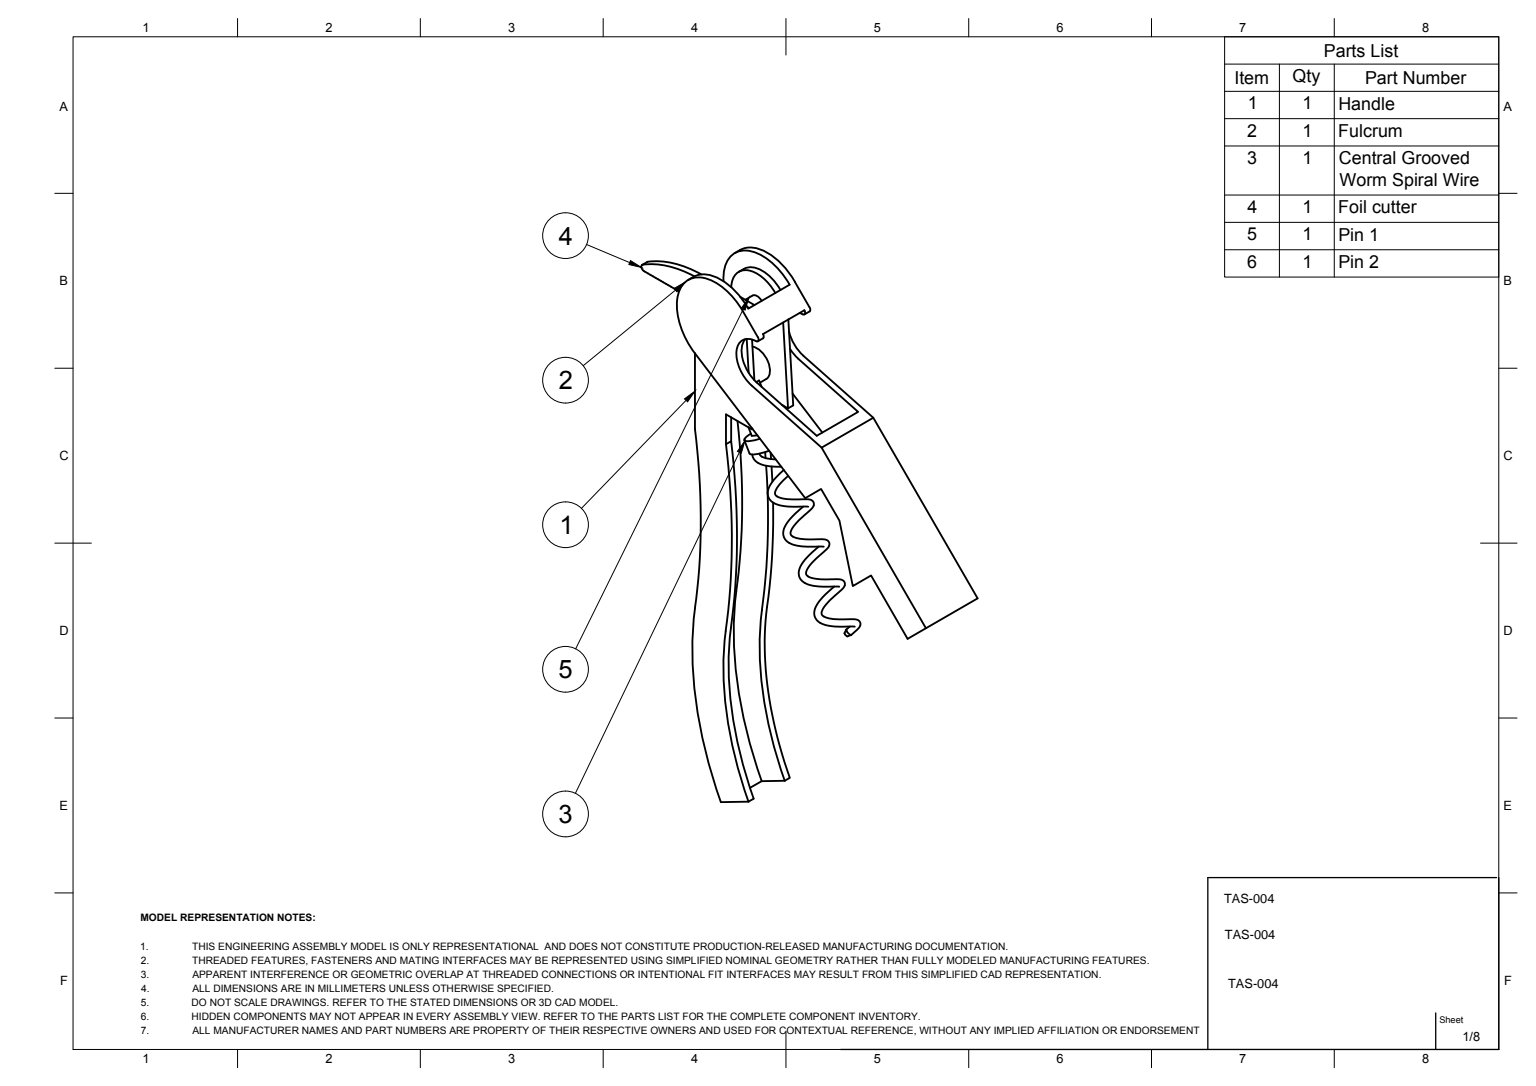
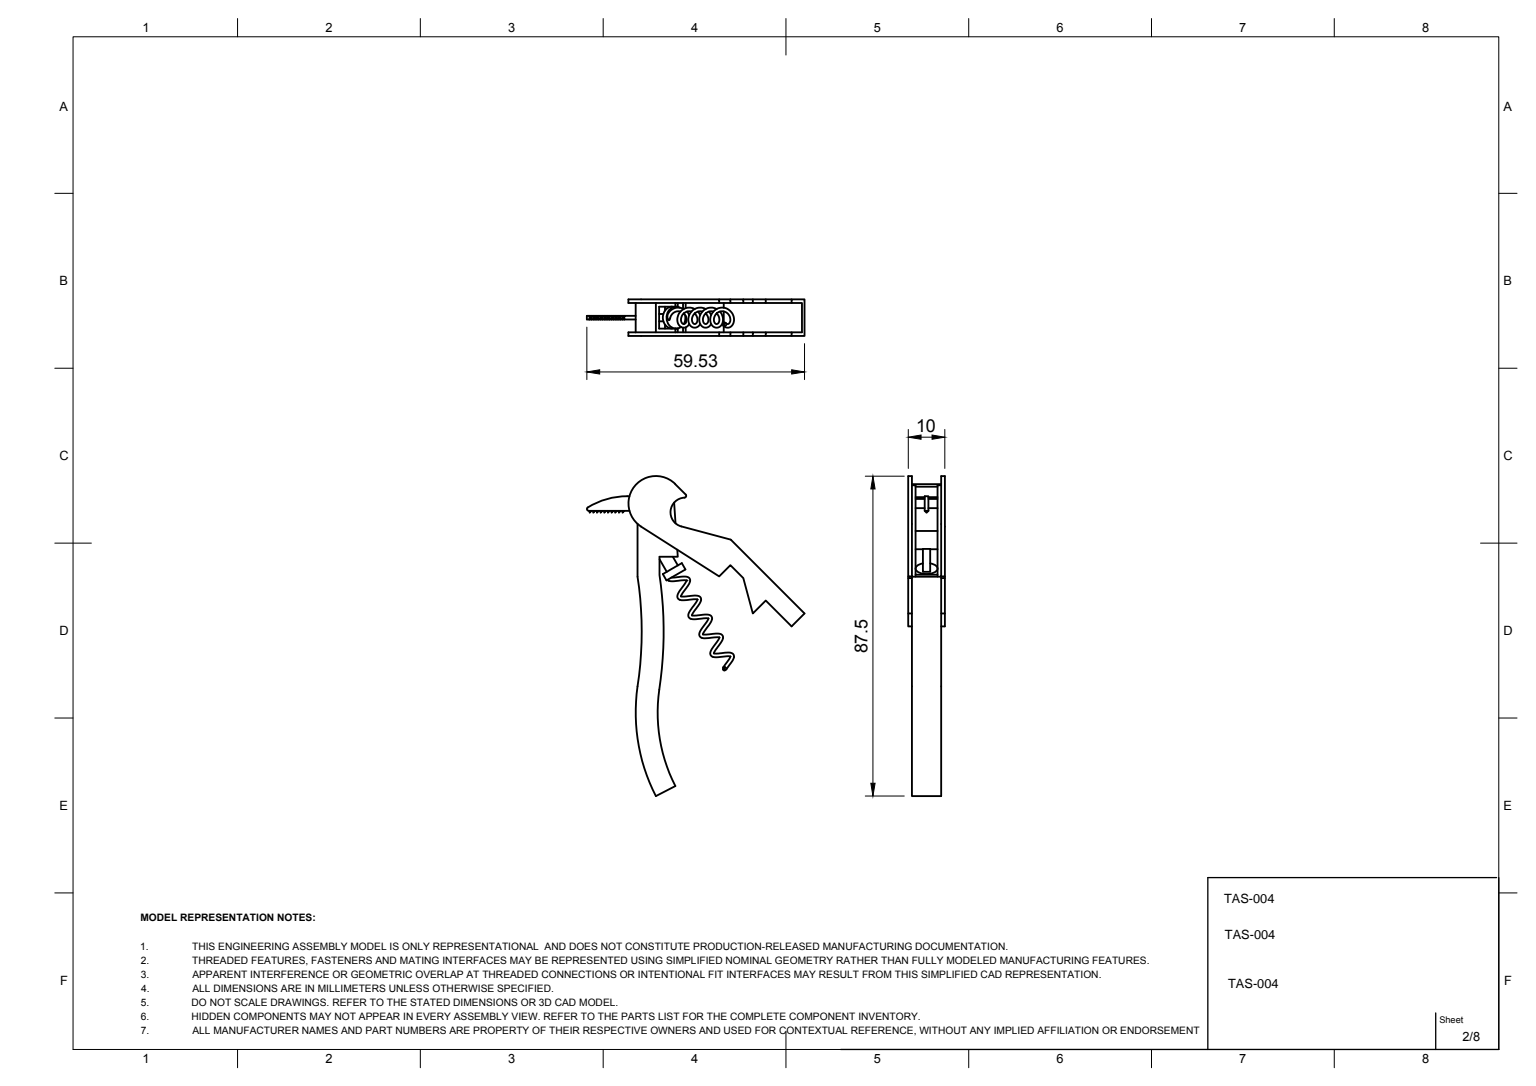
ISO-10303-21;
HEADER;
/* Generated by software containing ST-Developer
 * from STEP Tools, Inc. (www.steptools.com) 
 */

FILE_DESCRIPTION(
/* description */ ('STEP AP214'),
/* implementation_level */ '2;1');

FILE_NAME(
/* name */ 'TAS-004',
/* time_stamp */ '2026-11-04T19:48:07-08:00',
/* author */ (''),
/* organization */ (''),
/* preprocessor_version */ 'ST-DEVELOPER v20.2',
/* originating_system */ 'Autodesk Translation Framework v15.17.0.0',
/* authorisation */ '');

FILE_SCHEMA (('AUTOMOTIVE_DESIGN { 1 0 10303 214 3 1 1 }'));
ENDSEC;

DATA;
#10=MECHANICAL_DESIGN_GEOMETRIC_PRESENTATION_REPRESENTATION('',(#59,#60,
#61,#62,#63,#64),#9561);
#11=ITEM_DEFINED_TRANSFORMATION($,$,#2479,#2690);
#12=ITEM_DEFINED_TRANSFORMATION($,$,#2539,#2691);
#13=ITEM_DEFINED_TRANSFORMATION($,$,#2590,#2692);
#14=ITEM_DEFINED_TRANSFORMATION($,$,#2613,#2693);
#15=ITEM_DEFINED_TRANSFORMATION($,$,#2678,#2694);
#16=ITEM_DEFINED_TRANSFORMATION($,$,#2684,#2695);
#17=(
REPRESENTATION_RELATIONSHIP($,$,#9587,#9586)
REPRESENTATION_RELATIONSHIP_WITH_TRANSFORMATION(#11)
SHAPE_REPRESENTATION_RELATIONSHIP()
);
#18=(
REPRESENTATION_RELATIONSHIP($,$,#9588,#9586)
REPRESENTATION_RELATIONSHIP_WITH_TRANSFORMATION(#12)
SHAPE_REPRESENTATION_RELATIONSHIP()
);
#19=(
REPRESENTATION_RELATIONSHIP($,$,#9589,#9586)
REPRESENTATION_RELATIONSHIP_WITH_TRANSFORMATION(#13)
SHAPE_REPRESENTATION_RELATIONSHIP()
);
#20=(
REPRESENTATION_RELATIONSHIP($,$,#9590,#9586)
REPRESENTATION_RELATIONSHIP_WITH_TRANSFORMATION(#14)
SHAPE_REPRESENTATION_RELATIONSHIP()
);
#21=(
REPRESENTATION_RELATIONSHIP($,$,#9591,#9586)
REPRESENTATION_RELATIONSHIP_WITH_TRANSFORMATION(#15)
SHAPE_REPRESENTATION_RELATIONSHIP()
);
#22=(
REPRESENTATION_RELATIONSHIP($,$,#9592,#9586)
REPRESENTATION_RELATIONSHIP_WITH_TRANSFORMATION(#16)
SHAPE_REPRESENTATION_RELATIONSHIP()
);
#23=CONTEXT_DEPENDENT_SHAPE_REPRESENTATION(#17,#9580);
#24=CONTEXT_DEPENDENT_SHAPE_REPRESENTATION(#18,#9581);
#25=CONTEXT_DEPENDENT_SHAPE_REPRESENTATION(#19,#9582);
#26=CONTEXT_DEPENDENT_SHAPE_REPRESENTATION(#20,#9583);
#27=CONTEXT_DEPENDENT_SHAPE_REPRESENTATION(#21,#9584);
#28=CONTEXT_DEPENDENT_SHAPE_REPRESENTATION(#22,#9585);
#29=NEXT_ASSEMBLY_USAGE_OCCURRENCE('Handle:1','Handle:1','Handle:1',#9594,
#9595,'Handle:1');
#30=NEXT_ASSEMBLY_USAGE_OCCURRENCE('fulcrum:1','fulcrum:1','fulcrum:1',
#9594,#9596,'fulcrum:1');
#31=NEXT_ASSEMBLY_USAGE_OCCURRENCE('Central Grooved Worm Spiral Wire:1',
'Central Grooved Worm Spiral Wire:1',
'Central Grooved Worm Spiral Wire:1',#9594,#9597,
'Central Grooved Worm Spiral Wire:1');
#32=NEXT_ASSEMBLY_USAGE_OCCURRENCE('foil cutter:1','foil cutter:1',
'foil cutter:1',#9594,#9598,'foil cutter:1');
#33=NEXT_ASSEMBLY_USAGE_OCCURRENCE('pin 1:1','pin 1:1','pin 1:1',#9594,
#9599,'pin 1:1');
#34=NEXT_ASSEMBLY_USAGE_OCCURRENCE('pin 2:1','pin 2:1','pin 2:1',#9594,
#9600,'pin 2:1');
#35=(
BOUNDED_SURFACE()
B_SPLINE_SURFACE(3,2,((#4268,#4269,#4270,#4271,#4272,#4273,#4274,#4275,
#4276,#4277,#4278,#4279,#4280,#4281,#4282,#4283,#4284,#4285,#4286,#4287,
#4288,#4289,#4290,#4291,#4292,#4293,#4294,#4295,#4296,#4297,#4298,#4299,
#4300,#4301,#4302,#4303,#4304,#4305,#4306,#4307,#4308,#4309,#4310,#4311,
#4312,#4313,#4314,#4315,#4316,#4317,#4318,#4319,#4320,#4321,#4322,#4323,
#4324,#4325,#4326,#4327,#4328,#4329,#4330,#4331,#4332,#4333,#4334,#4335,
#4336,#4337,#4338,#4339,#4340,#4341,#4342,#4343,#4344,#4345,#4346,#4347,
#4348,#4349,#4350,#4351,#4352,#4353,#4354,#4355,#4356,#4357,#4358,#4359,
#4360,#4361,#4362,#4363,#4364,#4365,#4366,#4367,#4368,#4369,#4370,#4371,
#4372,#4373,#4374,#4375,#4376,#4377,#4378,#4379,#4380,#4381,#4382,#4383,
#4384,#4385,#4386,#4387,#4388,#4389,#4390,#4391,#4392,#4393,#4394,#4395,
#4396,#4397,#4398,#4399,#4400,#4401,#4402,#4403,#4404,#4405,#4406,#4407,
#4408),(#4409,#4410,#4411,#4412,#4413,#4414,#4415,#4416,#4417,#4418,#4419,
#4420,#4421,#4422,#4423,#4424,#4425,#4426,#4427,#4428,#4429,#4430,#4431,
#4432,#4433,#4434,#4435,#4436,#4437,#4438,#4439,#4440,#4441,#4442,#4443,
#4444,#4445,#4446,#4447,#4448,#4449,#4450,#4451,#4452,#4453,#4454,#4455,
#4456,#4457,#4458,#4459,#4460,#4461,#4462,#4463,#4464,#4465,#4466,#4467,
#4468,#4469,#4470,#4471,#4472,#4473,#4474,#4475,#4476,#4477,#4478,#4479,
#4480,#4481,#4482,#4483,#4484,#4485,#4486,#4487,#4488,#4489,#4490,#4491,
#4492,#4493,#4494,#4495,#4496,#4497,#4498,#4499,#4500,#4501,#4502,#4503,
#4504,#4505,#4506,#4507,#4508,#4509,#4510,#4511,#4512,#4513,#4514,#4515,
#4516,#4517,#4518,#4519,#4520,#4521,#4522,#4523,#4524,#4525,#4526,#4527,
#4528,#4529,#4530,#4531,#4532,#4533,#4534,#4535,#4536,#4537,#4538,#4539,
#4540,#4541,#4542,#4543,#4544,#4545,#4546,#4547,#4548,#4549),(#4550,#4551,
#4552,#4553,#4554,#4555,#4556,#4557,#4558,#4559,#4560,#4561,#4562,#4563,
#4564,#4565,#4566,#4567,#4568,#4569,#4570,#4571,#4572,#4573,#4574,#4575,
#4576,#4577,#4578,#4579,#4580,#4581,#4582,#4583,#4584,#4585,#4586,#4587,
#4588,#4589,#4590,#4591,#4592,#4593,#4594,#4595,#4596,#4597,#4598,#4599,
#4600,#4601,#4602,#4603,#4604,#4605,#4606,#4607,#4608,#4609,#4610,#4611,
#4612,#4613,#4614,#4615,#4616,#4617,#4618,#4619,#4620,#4621,#4622,#4623,
#4624,#4625,#4626,#4627,#4628,#4629,#4630,#4631,#4632,#4633,#4634,#4635,
#4636,#4637,#4638,#4639,#4640,#4641,#4642,#4643,#4644,#4645,#4646,#4647,
#4648,#4649,#4650,#4651,#4652,#4653,#4654,#4655,#4656,#4657,#4658,#4659,
#4660,#4661,#4662,#4663,#4664,#4665,#4666,#4667,#4668,#4669,#4670,#4671,
#4672,#4673,#4674,#4675,#4676,#4677,#4678,#4679,#4680,#4681,#4682,#4683,
#4684,#4685,#4686,#4687,#4688,#4689,#4690),(#4691,#4692,#4693,#4694,#4695,
#4696,#4697,#4698,#4699,#4700,#4701,#4702,#4703,#4704,#4705,#4706,#4707,
#4708,#4709,#4710,#4711,#4712,#4713,#4714,#4715,#4716,#4717,#4718,#4719,
#4720,#4721,#4722,#4723,#4724,#4725,#4726,#4727,#4728,#4729,#4730,#4731,
#4732,#4733,#4734,#4735,#4736,#4737,#4738,#4739,#4740,#4741,#4742,#4743,
#4744,#4745,#4746,#4747,#4748,#4749,#4750,#4751,#4752,#4753,#4754,#4755,
#4756,#4757,#4758,#4759,#4760,#4761,#4762,#4763,#4764,#4765,#4766,#4767,
#4768,#4769,#4770,#4771,#4772,#4773,#4774,#4775,#4776,#4777,#4778,#4779,
#4780,#4781,#4782,#4783,#4784,#4785,#4786,#4787,#4788,#4789,#4790,#4791,
#4792,#4793,#4794,#4795,#4796,#4797,#4798,#4799,#4800,#4801,#4802,#4803,
#4804,#4805,#4806,#4807,#4808,#4809,#4810,#4811,#4812,#4813,#4814,#4815,
#4816,#4817,#4818,#4819,#4820,#4821,#4822,#4823,#4824,#4825,#4826,#4827,
#4828,#4829,#4830,#4831),(#4832,#4833,#4834,#4835,#4836,#4837,#4838,#4839,
#4840,#4841,#4842,#4843,#4844,#4845,#4846,#4847,#4848,#4849,#4850,#4851,
#4852,#4853,#4854,#4855,#4856,#4857,#4858,#4859,#4860,#4861,#4862,#4863,
#4864,#4865,#4866,#4867,#4868,#4869,#4870,#4871,#4872,#4873,#4874,#4875,
#4876,#4877,#4878,#4879,#4880,#4881,#4882,#4883,#4884,#4885,#4886,#4887,
#4888,#4889,#4890,#4891,#4892,#4893,#4894,#4895,#4896,#4897,#4898,#4899,
#4900,#4901,#4902,#4903,#4904,#4905,#4906,#4907,#4908,#4909,#4910,#4911,
#4912,#4913,#4914,#4915,#4916,#4917,#4918,#4919,#4920,#4921,#4922,#4923,
#4924,#4925,#4926,#4927,#4928,#4929,#4930,#4931,#4932,#4933,#4934,#4935,
#4936,#4937,#4938,#4939,#4940,#4941,#4942,#4943,#4944,#4945,#4946,#4947,
#4948,#4949,#4950,#4951,#4952,#4953,#4954,#4955,#4956,#4957,#4958,#4959,
#4960,#4961,#4962,#4963,#4964,#4965,#4966,#4967,#4968,#4969,#4970,#4971,
#4972),(#4973,#4974,#4975,#4976,#4977,#4978,#4979,#4980,#4981,#4982,#4983,
#4984,#4985,#4986,#4987,#4988,#4989,#4990,#4991,#4992,#4993,#4994,#4995,
#4996,#4997,#4998,#4999,#5000,#5001,#5002,#5003,#5004,#5005,#5006,#5007,
#5008,#5009,#5010,#5011,#5012,#5013,#5014,#5015,#5016,#5017,#5018,#5019,
#5020,#5021,#5022,#5023,#5024,#5025,#5026,#5027,#5028,#5029,#5030,#5031,
#5032,#5033,#5034,#5035,#5036,#5037,#5038,#5039,#5040,#5041,#5042,#5043,
#5044,#5045,#5046,#5047,#5048,#5049,#5050,#5051,#5052,#5053,#5054,#5055,
#5056,#5057,#5058,#5059,#5060,#5061,#5062,#5063,#5064,#5065,#5066,#5067,
#5068,#5069,#5070,#5071,#5072,#5073,#5074,#5075,#5076,#5077,#5078,#5079,
#5080,#5081,#5082,#5083,#5084,#5085,#5086,#5087,#5088,#5089,#5090,#5091,
#5092,#5093,#5094,#5095,#5096,#5097,#5098,#5099,#5100,#5101,#5102,#5103,
#5104,#5105,#5106,#5107,#5108,#5109,#5110,#5111,#5112,#5113),(#5114,#5115,
#5116,#5117,#5118,#5119,#5120,#5121,#5122,#5123,#5124,#5125,#5126,#5127,
#5128,#5129,#5130,#5131,#5132,#5133,#5134,#5135,#5136,#5137,#5138,#5139,
#5140,#5141,#5142,#5143,#5144,#5145,#5146,#5147,#5148,#5149,#5150,#5151,
#5152,#5153,#5154,#5155,#5156,#5157,#5158,#5159,#5160,#5161,#5162,#5163,
#5164,#5165,#5166,#5167,#5168,#5169,#5170,#5171,#5172,#5173,#5174,#5175,
#5176,#5177,#5178,#5179,#5180,#5181,#5182,#5183,#5184,#5185,#5186,#5187,
#5188,#5189,#5190,#5191,#5192,#5193,#5194,#5195,#5196,#5197,#5198,#5199,
#5200,#5201,#5202,#5203,#5204,#5205,#5206,#5207,#5208,#5209,#5210,#5211,
#5212,#5213,#5214,#5215,#5216,#5217,#5218,#5219,#5220,#5221,#5222,#5223,
#5224,#5225,#5226,#5227,#5228,#5229,#5230,#5231,#5232,#5233,#5234,#5235,
#5236,#5237,#5238,#5239,#5240,#5241,#5242,#5243,#5244,#5245,#5246,#5247,
#5248,#5249,#5250,#5251,#5252,#5253,#5254)),.UNSPECIFIED.,.T.,.F.,.F.)
B_SPLINE_SURFACE_WITH_KNOTS((4,3,4),(3,2,2,2,2,2,2,2,2,2,2,2,2,2,2,2,2,
2,2,2,2,2,2,2,2,2,2,2,2,2,2,2,2,2,2,2,2,2,2,2,2,2,2,2,2,2,2,2,2,2,2,2,2,
2,2,2,2,2,2,2,2,2,2,2,2,2,2,2,2,2,3),(0.,0.5,1.),(0.,0.0142857142857143,
0.0285714285714286,0.0428571428571429,0.0571428571428571,0.0714285714285714,
0.0857142857142857,0.1,0.114285714285714,0.128571428571429,0.142857142857143,
0.157142857142857,0.171428571428571,0.185714285714286,0.2,0.214285714285714,
0.228571428571429,0.242857142857143,0.257142857142857,0.271428571428571,
0.285714285714286,0.3,0.314285714285714,0.328571428571429,0.342857142857143,
0.357142857142857,0.371428571428571,0.385714285714286,0.4,0.414285714285714,
0.428571428571429,0.442857142857143,0.457142857142857,0.471428571428571,
0.485714285714286,0.5,0.514285714285714,0.528571428571429,0.542857142857143,
0.557142857142857,0.571428571428571,0.585714285714286,0.6,0.614285714285714,
0.628571428571429,0.642857142857143,0.657142857142857,0.671428571428571,
0.685714285714286,0.7,0.714285714285714,0.728571428571429,0.742857142857143,
0.757142857142857,0.771428571428571,0.785714285714286,0.8,0.814285714285714,
0.828571428571429,0.842857142857143,0.857142857142857,0.871428571428571,
0.885714285714286,0.9,0.914285714285714,0.928571428571429,0.942857142857143,
0.957142857142857,0.971428571428571,0.985714285714286,1.),.UNSPECIFIED.)
GEOMETRIC_REPRESENTATION_ITEM()
RATIONAL_B_SPLINE_SURFACE(((1.,0.974927912181824,1.,0.974927912181824,1.,
0.974927912181824,1.,0.974927912181824,1.,0.974927912181824,1.,0.974927912181824,
1.,0.974927912181824,1.,0.974927912181824,1.,0.974927912181824,1.,0.974927912181824,
1.,0.974927912181824,1.,0.974927912181824,1.,0.974927912181824,1.,0.974927912181824,
1.,0.974927912181824,1.,0.974927912181824,1.,0.974927912181824,1.,0.974927912181824,
1.,0.974927912181824,1.,0.974927912181824,1.,0.974927912181824,1.,0.974927912181824,
1.,0.974927912181824,1.,0.974927912181824,1.,0.974927912181824,1.,0.974927912181824,
1.,0.974927912181824,1.,0.974927912181824,1.,0.974927912181824,1.,0.974927912181824,
1.,0.974927912181824,1.,0.974927912181824,1.,0.974927912181824,1.,0.974927912181824,
1.,0.974927912181824,1.,0.974927912181824,1.,0.974927912181824,1.,0.974927912181824,
1.,0.974927912181824,1.,0.974927912181824,1.,0.974927912181824,1.,0.974927912181824,
1.,0.974927912181824,1.,0.974927912181824,1.,0.974927912181824,1.,0.974927912181824,
1.,0.974927912181824,1.,0.974927912181824,1.,0.974927912181824,1.,0.974927912181824,
1.,0.974927912181824,1.,0.974927912181824,1.,0.974927912181824,1.,0.974927912181824,
1.,0.974927912181824,1.,0.974927912181824,1.,0.974927912181824,1.,0.974927912181824,
1.,0.974927912181824,1.,0.974927912181824,1.,0.974927912181824,1.,0.974927912181824,
1.,0.974927912181824,1.,0.974927912181824,1.,0.974927912181824,1.,0.974927912181824,
1.,0.974927912181824,1.,0.974927912181824,1.,0.974927912181824,1.,0.974927912181824,
1.),(0.333333333333333,0.324975970727275,0.333333333333333,0.324975970727275,
0.333333333333333,0.324975970727275,0.333333333333333,0.324975970727275,
0.333333333333333,0.324975970727275,0.333333333333333,0.324975970727275,
0.333333333333333,0.324975970727275,0.333333333333333,0.324975970727275,
0.333333333333333,0.324975970727275,0.333333333333333,0.324975970727275,
0.333333333333333,0.324975970727275,0.333333333333333,0.324975970727275,
0.333333333333333,0.324975970727275,0.333333333333333,0.324975970727275,
0.333333333333333,0.324975970727275,0.333333333333333,0.324975970727275,
0.333333333333333,0.324975970727275,0.333333333333333,0.324975970727275,
0.333333333333333,0.324975970727275,0.333333333333333,0.324975970727275,
0.333333333333333,0.324975970727275,0.333333333333333,0.324975970727275,
0.333333333333333,0.324975970727275,0.333333333333333,0.324975970727275,
0.333333333333333,0.324975970727275,0.333333333333333,0.324975970727275,
0.333333333333333,0.324975970727275,0.333333333333333,0.324975970727275,
0.333333333333333,0.324975970727275,0.333333333333333,0.324975970727275,
0.333333333333333,0.324975970727275,0.333333333333333,0.324975970727275,
0.333333333333333,0.324975970727275,0.333333333333333,0.324975970727275,
0.333333333333333,0.324975970727275,0.333333333333333,0.324975970727275,
0.333333333333333,0.324975970727275,0.333333333333333,0.324975970727275,
0.333333333333333,0.324975970727275,0.333333333333333,0.324975970727275,
0.333333333333333,0.324975970727275,0.333333333333333,0.324975970727275,
0.333333333333333,0.324975970727275,0.333333333333333,0.324975970727275,
0.333333333333333,0.324975970727275,0.333333333333333,0.324975970727275,
0.333333333333333,0.324975970727275,0.333333333333333,0.324975970727275,
0.333333333333333,0.324975970727275,0.333333333333333,0.324975970727275,
0.333333333333333,0.324975970727275,0.333333333333333,0.324975970727275,
0.333333333333333,0.324975970727275,0.333333333333333,0.324975970727275,
0.333333333333333,0.324975970727275,0.333333333333333,0.324975970727275,
0.333333333333333,0.324975970727275,0.333333333333333,0.324975970727275,
0.333333333333333,0.324975970727275,0.333333333333333,0.324975970727275,
0.333333333333333,0.324975970727275,0.333333333333333,0.324975970727275,
0.333333333333333,0.324975970727275,0.333333333333333,0.324975970727275,
0.333333333333333,0.324975970727275,0.333333333333333,0.324975970727275,
0.333333333333333,0.324975970727275,0.333333333333333,0.324975970727275,
0.333333333333333,0.324975970727275,0.333333333333333,0.324975970727275,
0.333333333333333),(0.333333333333333,0.324975970727275,0.333333333333333,
0.324975970727275,0.333333333333333,0.324975970727275,0.333333333333333,
0.324975970727275,0.333333333333333,0.324975970727275,0.333333333333333,
0.324975970727275,0.333333333333333,0.324975970727275,0.333333333333333,
0.324975970727275,0.333333333333333,0.324975970727275,0.333333333333333,
0.324975970727275,0.333333333333333,0.324975970727275,0.333333333333333,
0.324975970727275,0.333333333333333,0.324975970727275,0.333333333333333,
0.324975970727275,0.333333333333333,0.324975970727275,0.333333333333333,
0.324975970727275,0.333333333333333,0.324975970727275,0.333333333333333,
0.324975970727275,0.333333333333333,0.324975970727275,0.333333333333333,
0.324975970727275,0.333333333333333,0.324975970727275,0.333333333333333,
0.324975970727275,0.333333333333333,0.324975970727275,0.333333333333333,
0.324975970727275,0.333333333333333,0.324975970727275,0.333333333333333,
0.324975970727275,0.333333333333333,0.324975970727275,0.333333333333333,
0.324975970727275,0.333333333333333,0.324975970727275,0.333333333333333,
0.324975970727275,0.333333333333333,0.324975970727275,0.333333333333333,
0.324975970727275,0.333333333333333,0.324975970727275,0.333333333333333,
0.324975970727275,0.333333333333333,0.324975970727275,0.333333333333333,
0.324975970727275,0.333333333333333,0.324975970727275,0.333333333333333,
0.324975970727275,0.333333333333333,0.324975970727275,0.333333333333333,
0.324975970727275,0.333333333333333,0.324975970727275,0.333333333333333,
0.324975970727275,0.333333333333333,0.324975970727275,0.333333333333333,
0.324975970727275,0.333333333333333,0.324975970727275,0.333333333333333,
0.324975970727275,0.333333333333333,0.324975970727275,0.333333333333333,
0.324975970727275,0.333333333333333,0.324975970727275,0.333333333333333,
0.324975970727275,0.333333333333333,0.324975970727275,0.333333333333333,
0.324975970727275,0.333333333333333,0.324975970727275,0.333333333333333,
0.324975970727275,0.333333333333333,0.324975970727275,0.333333333333333,
0.324975970727275,0.333333333333333,0.324975970727275,0.333333333333333,
0.324975970727275,0.333333333333333,0.324975970727275,0.333333333333333,
0.324975970727275,0.333333333333333,0.324975970727275,0.333333333333333,
0.324975970727275,0.333333333333333,0.324975970727275,0.333333333333333,
0.324975970727275,0.333333333333333,0.324975970727275,0.333333333333333,
0.324975970727275,0.333333333333333,0.324975970727275,0.333333333333333,
0.324975970727275,0.333333333333333,0.324975970727275,0.333333333333333,
0.324975970727275,0.333333333333333),(1.,0.974927912181824,1.,0.974927912181824,
1.,0.974927912181824,1.,0.974927912181824,1.,0.974927912181824,1.,0.974927912181824,
1.,0.974927912181824,1.,0.974927912181824,1.,0.974927912181824,1.,0.974927912181824,
1.,0.974927912181824,1.,0.974927912181824,1.,0.974927912181824,1.,0.974927912181824,
1.,0.974927912181824,1.,0.974927912181824,1.,0.974927912181824,1.,0.974927912181824,
1.,0.974927912181824,1.,0.974927912181824,1.,0.974927912181824,1.,0.974927912181824,
1.,0.974927912181824,1.,0.974927912181824,1.,0.974927912181824,1.,0.974927912181824,
1.,0.974927912181824,1.,0.974927912181824,1.,0.974927912181824,1.,0.974927912181824,
1.,0.974927912181824,1.,0.974927912181824,1.,0.974927912181824,1.,0.974927912181824,
1.,0.974927912181824,1.,0.974927912181824,1.,0.974927912181824,1.,0.974927912181824,
1.,0.974927912181824,1.,0.974927912181824,1.,0.974927912181824,1.,0.974927912181824,
1.,0.974927912181824,1.,0.974927912181824,1.,0.974927912181824,1.,0.974927912181824,
1.,0.974927912181824,1.,0.974927912181824,1.,0.974927912181824,1.,0.974927912181824,
1.,0.974927912181824,1.,0.974927912181824,1.,0.974927912181824,1.,0.974927912181824,
1.,0.974927912181824,1.,0.974927912181824,1.,0.974927912181824,1.,0.974927912181824,
1.,0.974927912181824,1.,0.974927912181824,1.,0.974927912181824,1.,0.974927912181824,
1.,0.974927912181824,1.,0.974927912181824,1.,0.974927912181824,1.,0.974927912181824,
1.,0.974927912181824,1.,0.974927912181824,1.,0.974927912181824,1.,0.974927912181824,
1.),(0.333333333333333,0.324975970727275,0.333333333333333,0.324975970727275,
0.333333333333333,0.324975970727275,0.333333333333333,0.324975970727275,
0.333333333333333,0.324975970727275,0.333333333333333,0.324975970727275,
0.333333333333333,0.324975970727275,0.333333333333333,0.324975970727275,
0.333333333333333,0.324975970727275,0.333333333333333,0.324975970727275,
0.333333333333333,0.324975970727275,0.333333333333333,0.324975970727275,
0.333333333333333,0.324975970727275,0.333333333333333,0.324975970727275,
0.333333333333333,0.324975970727275,0.333333333333333,0.324975970727275,
0.333333333333333,0.324975970727275,0.333333333333333,0.324975970727275,
0.333333333333333,0.324975970727275,0.333333333333333,0.324975970727275,
0.333333333333333,0.324975970727275,0.333333333333333,0.324975970727275,
0.333333333333333,0.324975970727275,0.333333333333333,0.324975970727275,
0.333333333333333,0.324975970727275,0.333333333333333,0.324975970727275,
0.333333333333333,0.324975970727275,0.333333333333333,0.324975970727275,
0.333333333333333,0.324975970727275,0.333333333333333,0.324975970727275,
0.333333333333333,0.324975970727275,0.333333333333333,0.324975970727275,
0.333333333333333,0.324975970727275,0.333333333333333,0.324975970727275,
0.333333333333333,0.324975970727275,0.333333333333333,0.324975970727275,
0.333333333333333,0.324975970727275,0.333333333333333,0.324975970727275,
0.333333333333333,0.324975970727275,0.333333333333333,0.324975970727275,
0.333333333333333,0.324975970727275,0.333333333333333,0.324975970727275,
0.333333333333333,0.324975970727275,0.333333333333333,0.324975970727275,
0.333333333333333,0.324975970727275,0.333333333333333,0.324975970727275,
0.333333333333333,0.324975970727275,0.333333333333333,0.324975970727275,
0.333333333333333,0.324975970727275,0.333333333333333,0.324975970727275,
0.333333333333333,0.324975970727275,0.333333333333333,0.324975970727275,
0.333333333333333,0.324975970727275,0.333333333333333,0.324975970727275,
0.333333333333333,0.324975970727275,0.333333333333333,0.324975970727275,
0.333333333333333,0.324975970727275,0.333333333333333,0.324975970727275,
0.333333333333333,0.324975970727275,0.333333333333333,0.324975970727275,
0.333333333333333,0.324975970727275,0.333333333333333,0.324975970727275,
0.333333333333333,0.324975970727275,0.333333333333333,0.324975970727275,
0.333333333333333,0.324975970727275,0.333333333333333,0.324975970727275,
0.333333333333333,0.324975970727275,0.333333333333333,0.324975970727275,
0.333333333333333,0.324975970727275,0.333333333333333,0.324975970727275,
0.333333333333333),(0.333333333333333,0.324975970727275,0.333333333333333,
0.324975970727275,0.333333333333333,0.324975970727275,0.333333333333333,
0.324975970727275,0.333333333333333,0.324975970727275,0.333333333333333,
0.324975970727275,0.333333333333333,0.324975970727275,0.333333333333333,
0.324975970727275,0.333333333333333,0.324975970727275,0.333333333333333,
0.324975970727275,0.333333333333333,0.324975970727275,0.333333333333333,
0.324975970727275,0.333333333333333,0.324975970727275,0.333333333333333,
0.324975970727275,0.333333333333333,0.324975970727275,0.333333333333333,
0.324975970727275,0.333333333333333,0.324975970727275,0.333333333333333,
0.324975970727275,0.333333333333333,0.324975970727275,0.333333333333333,
0.324975970727275,0.333333333333333,0.324975970727275,0.333333333333333,
0.324975970727275,0.333333333333333,0.324975970727275,0.333333333333333,
0.324975970727275,0.333333333333333,0.324975970727275,0.333333333333333,
0.324975970727275,0.333333333333333,0.324975970727275,0.333333333333333,
0.324975970727275,0.333333333333333,0.324975970727275,0.333333333333333,
0.324975970727275,0.333333333333333,0.324975970727275,0.333333333333333,
0.324975970727275,0.333333333333333,0.324975970727275,0.333333333333333,
0.324975970727275,0.333333333333333,0.324975970727275,0.333333333333333,
0.324975970727275,0.333333333333333,0.324975970727275,0.333333333333333,
0.324975970727275,0.333333333333333,0.324975970727275,0.333333333333333,
0.324975970727275,0.333333333333333,0.324975970727275,0.333333333333333,
0.324975970727275,0.333333333333333,0.324975970727275,0.333333333333333,
0.324975970727275,0.333333333333333,0.324975970727275,0.333333333333333,
0.324975970727275,0.333333333333333,0.324975970727275,0.333333333333333,
0.324975970727275,0.333333333333333,0.324975970727275,0.333333333333333,
0.324975970727275,0.333333333333333,0.324975970727275,0.333333333333333,
0.324975970727275,0.333333333333333,0.324975970727275,0.333333333333333,
0.324975970727275,0.333333333333333,0.324975970727275,0.333333333333333,
0.324975970727275,0.333333333333333,0.324975970727275,0.333333333333333,
0.324975970727275,0.333333333333333,0.324975970727275,0.333333333333333,
0.324975970727275,0.333333333333333,0.324975970727275,0.333333333333333,
0.324975970727275,0.333333333333333,0.324975970727275,0.333333333333333,
0.324975970727275,0.333333333333333,0.324975970727275,0.333333333333333,
0.324975970727275,0.333333333333333,0.324975970727275,0.333333333333333,
0.324975970727275,0.333333333333333,0.324975970727275,0.333333333333333,
0.324975970727275,0.333333333333333),(1.,0.974927912181824,1.,0.974927912181824,
1.,0.974927912181824,1.,0.974927912181824,1.,0.974927912181824,1.,0.974927912181824,
1.,0.974927912181824,1.,0.974927912181824,1.,0.974927912181824,1.,0.974927912181824,
1.,0.974927912181824,1.,0.974927912181824,1.,0.974927912181824,1.,0.974927912181824,
1.,0.974927912181824,1.,0.974927912181824,1.,0.974927912181824,1.,0.974927912181824,
1.,0.974927912181824,1.,0.974927912181824,1.,0.974927912181824,1.,0.974927912181824,
1.,0.974927912181824,1.,0.974927912181824,1.,0.974927912181824,1.,0.974927912181824,
1.,0.974927912181824,1.,0.974927912181824,1.,0.974927912181824,1.,0.974927912181824,
1.,0.974927912181824,1.,0.974927912181824,1.,0.974927912181824,1.,0.974927912181824,
1.,0.974927912181824,1.,0.974927912181824,1.,0.974927912181824,1.,0.974927912181824,
1.,0.974927912181824,1.,0.974927912181824,1.,0.974927912181824,1.,0.974927912181824,
1.,0.974927912181824,1.,0.974927912181824,1.,0.974927912181824,1.,0.974927912181824,
1.,0.974927912181824,1.,0.974927912181824,1.,0.974927912181824,1.,0.974927912181824,
1.,0.974927912181824,1.,0.974927912181824,1.,0.974927912181824,1.,0.974927912181824,
1.,0.974927912181824,1.,0.974927912181824,1.,0.974927912181824,1.,0.974927912181824,
1.,0.974927912181824,1.,0.974927912181824,1.,0.974927912181824,1.,0.974927912181824,
1.,0.974927912181824,1.,0.974927912181824,1.,0.974927912181824,1.,0.974927912181824,
1.,0.974927912181824,1.,0.974927912181824,1.,0.974927912181824,1.,0.974927912181824,
1.)))
REPRESENTATION_ITEM('')
SURFACE()
);
#36=(
BOUNDED_SURFACE()
B_SPLINE_SURFACE(3,2,((#8296,#8297,#8298,#8299,#8300,#8301,#8302,#8303,
#8304,#8305,#8306,#8307,#8308,#8309,#8310,#8311,#8312,#8313,#8314,#8315,
#8316,#8317,#8318,#8319,#8320,#8321,#8322,#8323,#8324,#8325,#8326,#8327,
#8328,#8329,#8330,#8331,#8332,#8333,#8334,#8335,#8336,#8337,#8338,#8339,
#8340,#8341,#8342,#8343,#8344,#8345,#8346,#8347,#8348,#8349,#8350,#8351,
#8352,#8353,#8354,#8355,#8356,#8357,#8358,#8359,#8360,#8361,#8362,#8363,
#8364,#8365,#8366,#8367,#8368,#8369,#8370,#8371,#8372,#8373,#8374,#8375,
#8376,#8377,#8378,#8379,#8380,#8381,#8382,#8383,#8384,#8385,#8386,#8387,
#8388,#8389,#8390,#8391,#8392,#8393,#8394,#8395,#8396,#8397,#8398,#8399,
#8400,#8401,#8402,#8403,#8404,#8405,#8406,#8407,#8408,#8409,#8410,#8411,
#8412,#8413,#8414,#8415,#8416,#8417,#8418,#8419,#8420,#8421,#8422,#8423,
#8424,#8425,#8426,#8427,#8428,#8429,#8430,#8431,#8432,#8433,#8434,#8435,
#8436),(#8437,#8438,#8439,#8440,#8441,#8442,#8443,#8444,#8445,#8446,#8447,
#8448,#8449,#8450,#8451,#8452,#8453,#8454,#8455,#8456,#8457,#8458,#8459,
#8460,#8461,#8462,#8463,#8464,#8465,#8466,#8467,#8468,#8469,#8470,#8471,
#8472,#8473,#8474,#8475,#8476,#8477,#8478,#8479,#8480,#8481,#8482,#8483,
#8484,#8485,#8486,#8487,#8488,#8489,#8490,#8491,#8492,#8493,#8494,#8495,
#8496,#8497,#8498,#8499,#8500,#8501,#8502,#8503,#8504,#8505,#8506,#8507,
#8508,#8509,#8510,#8511,#8512,#8513,#8514,#8515,#8516,#8517,#8518,#8519,
#8520,#8521,#8522,#8523,#8524,#8525,#8526,#8527,#8528,#8529,#8530,#8531,
#8532,#8533,#8534,#8535,#8536,#8537,#8538,#8539,#8540,#8541,#8542,#8543,
#8544,#8545,#8546,#8547,#8548,#8549,#8550,#8551,#8552,#8553,#8554,#8555,
#8556,#8557,#8558,#8559,#8560,#8561,#8562,#8563,#8564,#8565,#8566,#8567,
#8568,#8569,#8570,#8571,#8572,#8573,#8574,#8575,#8576,#8577),(#8578,#8579,
#8580,#8581,#8582,#8583,#8584,#8585,#8586,#8587,#8588,#8589,#8590,#8591,
#8592,#8593,#8594,#8595,#8596,#8597,#8598,#8599,#8600,#8601,#8602,#8603,
#8604,#8605,#8606,#8607,#8608,#8609,#8610,#8611,#8612,#8613,#8614,#8615,
#8616,#8617,#8618,#8619,#8620,#8621,#8622,#8623,#8624,#8625,#8626,#8627,
#8628,#8629,#8630,#8631,#8632,#8633,#8634,#8635,#8636,#8637,#8638,#8639,
#8640,#8641,#8642,#8643,#8644,#8645,#8646,#8647,#8648,#8649,#8650,#8651,
#8652,#8653,#8654,#8655,#8656,#8657,#8658,#8659,#8660,#8661,#8662,#8663,
#8664,#8665,#8666,#8667,#8668,#8669,#8670,#8671,#8672,#8673,#8674,#8675,
#8676,#8677,#8678,#8679,#8680,#8681,#8682,#8683,#8684,#8685,#8686,#8687,
#8688,#8689,#8690,#8691,#8692,#8693,#8694,#8695,#8696,#8697,#8698,#8699,
#8700,#8701,#8702,#8703,#8704,#8705,#8706,#8707,#8708,#8709,#8710,#8711,
#8712,#8713,#8714,#8715,#8716,#8717,#8718),(#8719,#8720,#8721,#8722,#8723,
#8724,#8725,#8726,#8727,#8728,#8729,#8730,#8731,#8732,#8733,#8734,#8735,
#8736,#8737,#8738,#8739,#8740,#8741,#8742,#8743,#8744,#8745,#8746,#8747,
#8748,#8749,#8750,#8751,#8752,#8753,#8754,#8755,#8756,#8757,#8758,#8759,
#8760,#8761,#8762,#8763,#8764,#8765,#8766,#8767,#8768,#8769,#8770,#8771,
#8772,#8773,#8774,#8775,#8776,#8777,#8778,#8779,#8780,#8781,#8782,#8783,
#8784,#8785,#8786,#8787,#8788,#8789,#8790,#8791,#8792,#8793,#8794,#8795,
#8796,#8797,#8798,#8799,#8800,#8801,#8802,#8803,#8804,#8805,#8806,#8807,
#8808,#8809,#8810,#8811,#8812,#8813,#8814,#8815,#8816,#8817,#8818,#8819,
#8820,#8821,#8822,#8823,#8824,#8825,#8826,#8827,#8828,#8829,#8830,#8831,
#8832,#8833,#8834,#8835,#8836,#8837,#8838,#8839,#8840,#8841,#8842,#8843,
#8844,#8845,#8846,#8847,#8848,#8849,#8850,#8851,#8852,#8853,#8854,#8855,
#8856,#8857,#8858,#8859),(#8860,#8861,#8862,#8863,#8864,#8865,#8866,#8867,
#8868,#8869,#8870,#8871,#8872,#8873,#8874,#8875,#8876,#8877,#8878,#8879,
#8880,#8881,#8882,#8883,#8884,#8885,#8886,#8887,#8888,#8889,#8890,#8891,
#8892,#8893,#8894,#8895,#8896,#8897,#8898,#8899,#8900,#8901,#8902,#8903,
#8904,#8905,#8906,#8907,#8908,#8909,#8910,#8911,#8912,#8913,#8914,#8915,
#8916,#8917,#8918,#8919,#8920,#8921,#8922,#8923,#8924,#8925,#8926,#8927,
#8928,#8929,#8930,#8931,#8932,#8933,#8934,#8935,#8936,#8937,#8938,#8939,
#8940,#8941,#8942,#8943,#8944,#8945,#8946,#8947,#8948,#8949,#8950,#8951,
#8952,#8953,#8954,#8955,#8956,#8957,#8958,#8959,#8960,#8961,#8962,#8963,
#8964,#8965,#8966,#8967,#8968,#8969,#8970,#8971,#8972,#8973,#8974,#8975,
#8976,#8977,#8978,#8979,#8980,#8981,#8982,#8983,#8984,#8985,#8986,#8987,
#8988,#8989,#8990,#8991,#8992,#8993,#8994,#8995,#8996,#8997,#8998,#8999,
#9000),(#9001,#9002,#9003,#9004,#9005,#9006,#9007,#9008,#9009,#9010,#9011,
#9012,#9013,#9014,#9015,#9016,#9017,#9018,#9019,#9020,#9021,#9022,#9023,
#9024,#9025,#9026,#9027,#9028,#9029,#9030,#9031,#9032,#9033,#9034,#9035,
#9036,#9037,#9038,#9039,#9040,#9041,#9042,#9043,#9044,#9045,#9046,#9047,
#9048,#9049,#9050,#9051,#9052,#9053,#9054,#9055,#9056,#9057,#9058,#9059,
#9060,#9061,#9062,#9063,#9064,#9065,#9066,#9067,#9068,#9069,#9070,#9071,
#9072,#9073,#9074,#9075,#9076,#9077,#9078,#9079,#9080,#9081,#9082,#9083,
#9084,#9085,#9086,#9087,#9088,#9089,#9090,#9091,#9092,#9093,#9094,#9095,
#9096,#9097,#9098,#9099,#9100,#9101,#9102,#9103,#9104,#9105,#9106,#9107,
#9108,#9109,#9110,#9111,#9112,#9113,#9114,#9115,#9116,#9117,#9118,#9119,
#9120,#9121,#9122,#9123,#9124,#9125,#9126,#9127,#9128,#9129,#9130,#9131,
#9132,#9133,#9134,#9135,#9136,#9137,#9138,#9139,#9140,#9141),(#9142,#9143,
#9144,#9145,#9146,#9147,#9148,#9149,#9150,#9151,#9152,#9153,#9154,#9155,
#9156,#9157,#9158,#9159,#9160,#9161,#9162,#9163,#9164,#9165,#9166,#9167,
#9168,#9169,#9170,#9171,#9172,#9173,#9174,#9175,#9176,#9177,#9178,#9179,
#9180,#9181,#9182,#9183,#9184,#9185,#9186,#9187,#9188,#9189,#9190,#9191,
#9192,#9193,#9194,#9195,#9196,#9197,#9198,#9199,#9200,#9201,#9202,#9203,
#9204,#9205,#9206,#9207,#9208,#9209,#9210,#9211,#9212,#9213,#9214,#9215,
#9216,#9217,#9218,#9219,#9220,#9221,#9222,#9223,#9224,#9225,#9226,#9227,
#9228,#9229,#9230,#9231,#9232,#9233,#9234,#9235,#9236,#9237,#9238,#9239,
#9240,#9241,#9242,#9243,#9244,#9245,#9246,#9247,#9248,#9249,#9250,#9251,
#9252,#9253,#9254,#9255,#9256,#9257,#9258,#9259,#9260,#9261,#9262,#9263,
#9264,#9265,#9266,#9267,#9268,#9269,#9270,#9271,#9272,#9273,#9274,#9275,
#9276,#9277,#9278,#9279,#9280,#9281,#9282)),.UNSPECIFIED.,.T.,.F.,.F.)
B_SPLINE_SURFACE_WITH_KNOTS((4,3,4),(3,2,2,2,2,2,2,2,2,2,2,2,2,2,2,2,2,
2,2,2,2,2,2,2,2,2,2,2,2,2,2,2,2,2,2,2,2,2,2,2,2,2,2,2,2,2,2,2,2,2,2,2,2,
2,2,2,2,2,2,2,2,2,2,2,2,2,2,2,2,2,3),(0.,0.5,1.),(0.,0.0142857142857143,
0.0285714285714286,0.0428571428571429,0.0571428571428571,0.0714285714285714,
0.0857142857142857,0.1,0.114285714285714,0.128571428571429,0.142857142857143,
0.157142857142857,0.171428571428571,0.185714285714286,0.2,0.214285714285714,
0.228571428571429,0.242857142857143,0.257142857142857,0.271428571428571,
0.285714285714286,0.3,0.314285714285714,0.328571428571429,0.342857142857143,
0.357142857142857,0.371428571428571,0.385714285714286,0.4,0.414285714285714,
0.428571428571429,0.442857142857143,0.457142857142857,0.471428571428571,
0.485714285714286,0.5,0.514285714285714,0.528571428571429,0.542857142857143,
0.557142857142857,0.571428571428571,0.585714285714286,0.6,0.614285714285714,
0.628571428571429,0.642857142857143,0.657142857142857,0.671428571428571,
0.685714285714286,0.7,0.714285714285714,0.728571428571429,0.742857142857143,
0.757142857142857,0.771428571428571,0.785714285714286,0.8,0.814285714285714,
0.828571428571429,0.842857142857143,0.857142857142857,0.871428571428571,
0.885714285714286,0.9,0.914285714285714,0.928571428571429,0.942857142857143,
0.957142857142857,0.971428571428571,0.985714285714286,1.),.UNSPECIFIED.)
GEOMETRIC_REPRESENTATION_ITEM()
RATIONAL_B_SPLINE_SURFACE(((1.,0.974927912181824,1.,0.974927912181824,1.,
0.974927912181824,1.,0.974927912181824,1.,0.974927912181824,1.,0.974927912181824,
1.,0.974927912181824,1.,0.974927912181824,1.,0.974927912181824,1.,0.974927912181824,
1.,0.974927912181824,1.,0.974927912181824,1.,0.974927912181824,1.,0.974927912181824,
1.,0.974927912181824,1.,0.974927912181824,1.,0.974927912181824,1.,0.974927912181824,
1.,0.974927912181824,1.,0.974927912181824,1.,0.974927912181824,1.,0.974927912181824,
1.,0.974927912181824,1.,0.974927912181824,1.,0.974927912181824,1.,0.974927912181824,
1.,0.974927912181824,1.,0.974927912181824,1.,0.974927912181824,1.,0.974927912181824,
1.,0.974927912181824,1.,0.974927912181824,1.,0.974927912181824,1.,0.974927912181824,
1.,0.974927912181824,1.,0.974927912181824,1.,0.974927912181824,1.,0.974927912181824,
1.,0.974927912181824,1.,0.974927912181824,1.,0.974927912181824,1.,0.974927912181824,
1.,0.974927912181824,1.,0.974927912181824,1.,0.974927912181824,1.,0.974927912181824,
1.,0.974927912181824,1.,0.974927912181824,1.,0.974927912181824,1.,0.974927912181824,
1.,0.974927912181824,1.,0.974927912181824,1.,0.974927912181824,1.,0.974927912181824,
1.,0.974927912181824,1.,0.974927912181824,1.,0.974927912181824,1.,0.974927912181824,
1.,0.974927912181824,1.,0.974927912181824,1.,0.974927912181824,1.,0.974927912181824,
1.,0.974927912181824,1.,0.974927912181824,1.,0.974927912181824,1.,0.974927912181824,
1.,0.974927912181824,1.,0.974927912181824,1.,0.974927912181824,1.,0.974927912181824,
1.),(0.333333333333333,0.324975970727275,0.333333333333333,0.324975970727275,
0.333333333333333,0.324975970727275,0.333333333333333,0.324975970727275,
0.333333333333333,0.324975970727275,0.333333333333333,0.324975970727275,
0.333333333333333,0.324975970727275,0.333333333333333,0.324975970727275,
0.333333333333333,0.324975970727275,0.333333333333333,0.324975970727275,
0.333333333333333,0.324975970727275,0.333333333333333,0.324975970727275,
0.333333333333333,0.324975970727275,0.333333333333333,0.324975970727275,
0.333333333333333,0.324975970727275,0.333333333333333,0.324975970727275,
0.333333333333333,0.324975970727275,0.333333333333333,0.324975970727275,
0.333333333333333,0.324975970727275,0.333333333333333,0.324975970727275,
0.333333333333333,0.324975970727275,0.333333333333333,0.324975970727275,
0.333333333333333,0.324975970727275,0.333333333333333,0.324975970727275,
0.333333333333333,0.324975970727275,0.333333333333333,0.324975970727275,
0.333333333333333,0.324975970727275,0.333333333333333,0.324975970727275,
0.333333333333333,0.324975970727275,0.333333333333333,0.324975970727275,
0.333333333333333,0.324975970727275,0.333333333333333,0.324975970727275,
0.333333333333333,0.324975970727275,0.333333333333333,0.324975970727275,
0.333333333333333,0.324975970727275,0.333333333333333,0.324975970727275,
0.333333333333333,0.324975970727275,0.333333333333333,0.324975970727275,
0.333333333333333,0.324975970727275,0.333333333333333,0.324975970727275,
0.333333333333333,0.324975970727275,0.333333333333333,0.324975970727275,
0.333333333333333,0.324975970727275,0.333333333333333,0.324975970727275,
0.333333333333333,0.324975970727275,0.333333333333333,0.324975970727275,
0.333333333333333,0.324975970727275,0.333333333333333,0.324975970727275,
0.333333333333333,0.324975970727275,0.333333333333333,0.324975970727275,
0.333333333333333,0.324975970727275,0.333333333333333,0.324975970727275,
0.333333333333333,0.324975970727275,0.333333333333333,0.324975970727275,
0.333333333333333,0.324975970727275,0.333333333333333,0.324975970727275,
0.333333333333333,0.324975970727275,0.333333333333333,0.324975970727275,
0.333333333333333,0.324975970727275,0.333333333333333,0.324975970727275,
0.333333333333333,0.324975970727275,0.333333333333333,0.324975970727275,
0.333333333333333,0.324975970727275,0.333333333333333,0.324975970727275,
0.333333333333333,0.324975970727275,0.333333333333333,0.324975970727275,
0.333333333333333,0.324975970727275,0.333333333333333,0.324975970727275,
0.333333333333333,0.324975970727275,0.333333333333333,0.324975970727275,
0.333333333333333),(0.333333333333333,0.324975970727275,0.333333333333333,
0.324975970727275,0.333333333333333,0.324975970727275,0.333333333333333,
0.324975970727275,0.333333333333333,0.324975970727275,0.333333333333333,
0.324975970727275,0.333333333333333,0.324975970727275,0.333333333333333,
0.324975970727275,0.333333333333333,0.324975970727275,0.333333333333333,
0.324975970727275,0.333333333333333,0.324975970727275,0.333333333333333,
0.324975970727275,0.333333333333333,0.324975970727275,0.333333333333333,
0.324975970727275,0.333333333333333,0.324975970727275,0.333333333333333,
0.324975970727275,0.333333333333333,0.324975970727275,0.333333333333333,
0.324975970727275,0.333333333333333,0.324975970727275,0.333333333333333,
0.324975970727275,0.333333333333333,0.324975970727275,0.333333333333333,
0.324975970727275,0.333333333333333,0.324975970727275,0.333333333333333,
0.324975970727275,0.333333333333333,0.324975970727275,0.333333333333333,
0.324975970727275,0.333333333333333,0.324975970727275,0.333333333333333,
0.324975970727275,0.333333333333333,0.324975970727275,0.333333333333333,
0.324975970727275,0.333333333333333,0.324975970727275,0.333333333333333,
0.324975970727275,0.333333333333333,0.324975970727275,0.333333333333333,
0.324975970727275,0.333333333333333,0.324975970727275,0.333333333333333,
0.324975970727275,0.333333333333333,0.324975970727275,0.333333333333333,
0.324975970727275,0.333333333333333,0.324975970727275,0.333333333333333,
0.324975970727275,0.333333333333333,0.324975970727275,0.333333333333333,
0.324975970727275,0.333333333333333,0.324975970727275,0.333333333333333,
0.324975970727275,0.333333333333333,0.324975970727275,0.333333333333333,
0.324975970727275,0.333333333333333,0.324975970727275,0.333333333333333,
0.324975970727275,0.333333333333333,0.324975970727275,0.333333333333333,
0.324975970727275,0.333333333333333,0.324975970727275,0.333333333333333,
0.324975970727275,0.333333333333333,0.324975970727275,0.333333333333333,
0.324975970727275,0.333333333333333,0.324975970727275,0.333333333333333,
0.324975970727275,0.333333333333333,0.324975970727275,0.333333333333333,
0.324975970727275,0.333333333333333,0.324975970727275,0.333333333333333,
0.324975970727275,0.333333333333333,0.324975970727275,0.333333333333333,
0.324975970727275,0.333333333333333,0.324975970727275,0.333333333333333,
0.324975970727275,0.333333333333333,0.324975970727275,0.333333333333333,
0.324975970727275,0.333333333333333,0.324975970727275,0.333333333333333,
0.324975970727275,0.333333333333333,0.324975970727275,0.333333333333333,
0.324975970727275,0.333333333333333),(1.,0.974927912181824,1.,0.974927912181824,
1.,0.974927912181824,1.,0.974927912181824,1.,0.974927912181824,1.,0.974927912181824,
1.,0.974927912181824,1.,0.974927912181824,1.,0.974927912181824,1.,0.974927912181824,
1.,0.974927912181824,1.,0.974927912181824,1.,0.974927912181824,1.,0.974927912181824,
1.,0.974927912181824,1.,0.974927912181824,1.,0.974927912181824,1.,0.974927912181824,
1.,0.974927912181824,1.,0.974927912181824,1.,0.974927912181824,1.,0.974927912181824,
1.,0.974927912181824,1.,0.974927912181824,1.,0.974927912181824,1.,0.974927912181824,
1.,0.974927912181824,1.,0.974927912181824,1.,0.974927912181824,1.,0.974927912181824,
1.,0.974927912181824,1.,0.974927912181824,1.,0.974927912181824,1.,0.974927912181824,
1.,0.974927912181824,1.,0.974927912181824,1.,0.974927912181824,1.,0.974927912181824,
1.,0.974927912181824,1.,0.974927912181824,1.,0.974927912181824,1.,0.974927912181824,
1.,0.974927912181824,1.,0.974927912181824,1.,0.974927912181824,1.,0.974927912181824,
1.,0.974927912181824,1.,0.974927912181824,1.,0.974927912181824,1.,0.974927912181824,
1.,0.974927912181824,1.,0.974927912181824,1.,0.974927912181824,1.,0.974927912181824,
1.,0.974927912181824,1.,0.974927912181824,1.,0.974927912181824,1.,0.974927912181824,
1.,0.974927912181824,1.,0.974927912181824,1.,0.974927912181824,1.,0.974927912181824,
1.,0.974927912181824,1.,0.974927912181824,1.,0.974927912181824,1.,0.974927912181824,
1.,0.974927912181824,1.,0.974927912181824,1.,0.974927912181824,1.,0.974927912181824,
1.),(0.333333333333333,0.324975970727275,0.333333333333333,0.324975970727275,
0.333333333333333,0.324975970727275,0.333333333333333,0.324975970727275,
0.333333333333333,0.324975970727275,0.333333333333333,0.324975970727275,
0.333333333333333,0.324975970727275,0.333333333333333,0.324975970727275,
0.333333333333333,0.324975970727275,0.333333333333333,0.324975970727275,
0.333333333333333,0.324975970727275,0.333333333333333,0.324975970727275,
0.333333333333333,0.324975970727275,0.333333333333333,0.324975970727275,
0.333333333333333,0.324975970727275,0.333333333333333,0.324975970727275,
0.333333333333333,0.324975970727275,0.333333333333333,0.324975970727275,
0.333333333333333,0.324975970727275,0.333333333333333,0.324975970727275,
0.333333333333333,0.324975970727275,0.333333333333333,0.324975970727275,
0.333333333333333,0.324975970727275,0.333333333333333,0.324975970727275,
0.333333333333333,0.324975970727275,0.333333333333333,0.324975970727275,
0.333333333333333,0.324975970727275,0.333333333333333,0.324975970727275,
0.333333333333333,0.324975970727275,0.333333333333333,0.324975970727275,
0.333333333333333,0.324975970727275,0.333333333333333,0.324975970727275,
0.333333333333333,0.324975970727275,0.333333333333333,0.324975970727275,
0.333333333333333,0.324975970727275,0.333333333333333,0.324975970727275,
0.333333333333333,0.324975970727275,0.333333333333333,0.324975970727275,
0.333333333333333,0.324975970727275,0.333333333333333,0.324975970727275,
0.333333333333333,0.324975970727275,0.333333333333333,0.324975970727275,
0.333333333333333,0.324975970727275,0.333333333333333,0.324975970727275,
0.333333333333333,0.324975970727275,0.333333333333333,0.324975970727275,
0.333333333333333,0.324975970727275,0.333333333333333,0.324975970727275,
0.333333333333333,0.324975970727275,0.333333333333333,0.324975970727275,
0.333333333333333,0.324975970727275,0.333333333333333,0.324975970727275,
0.333333333333333,0.324975970727275,0.333333333333333,0.324975970727275,
0.333333333333333,0.324975970727275,0.333333333333333,0.324975970727275,
0.333333333333333,0.324975970727275,0.333333333333333,0.324975970727275,
0.333333333333333,0.324975970727275,0.333333333333333,0.324975970727275,
0.333333333333333,0.324975970727275,0.333333333333333,0.324975970727275,
0.333333333333333,0.324975970727275,0.333333333333333,0.324975970727275,
0.333333333333333,0.324975970727275,0.333333333333333,0.324975970727275,
0.333333333333333,0.324975970727275,0.333333333333333,0.324975970727275,
0.333333333333333,0.324975970727275,0.333333333333333,0.324975970727275,
0.333333333333333),(0.333333333333333,0.324975970727275,0.333333333333333,
0.324975970727275,0.333333333333333,0.324975970727275,0.333333333333333,
0.324975970727275,0.333333333333333,0.324975970727275,0.333333333333333,
0.324975970727275,0.333333333333333,0.324975970727275,0.333333333333333,
0.324975970727275,0.333333333333333,0.324975970727275,0.333333333333333,
0.324975970727275,0.333333333333333,0.324975970727275,0.333333333333333,
0.324975970727275,0.333333333333333,0.324975970727275,0.333333333333333,
0.324975970727275,0.333333333333333,0.324975970727275,0.333333333333333,
0.324975970727275,0.333333333333333,0.324975970727275,0.333333333333333,
0.324975970727275,0.333333333333333,0.324975970727275,0.333333333333333,
0.324975970727275,0.333333333333333,0.324975970727275,0.333333333333333,
0.324975970727275,0.333333333333333,0.324975970727275,0.333333333333333,
0.324975970727275,0.333333333333333,0.324975970727275,0.333333333333333,
0.324975970727275,0.333333333333333,0.324975970727275,0.333333333333333,
0.324975970727275,0.333333333333333,0.324975970727275,0.333333333333333,
0.324975970727275,0.333333333333333,0.324975970727275,0.333333333333333,
0.324975970727275,0.333333333333333,0.324975970727275,0.333333333333333,
0.324975970727275,0.333333333333333,0.324975970727275,0.333333333333333,
0.324975970727275,0.333333333333333,0.324975970727275,0.333333333333333,
0.324975970727275,0.333333333333333,0.324975970727275,0.333333333333333,
0.324975970727275,0.333333333333333,0.324975970727275,0.333333333333333,
0.324975970727275,0.333333333333333,0.324975970727275,0.333333333333333,
0.324975970727275,0.333333333333333,0.324975970727275,0.333333333333333,
0.324975970727275,0.333333333333333,0.324975970727275,0.333333333333333,
0.324975970727275,0.333333333333333,0.324975970727275,0.333333333333333,
0.324975970727275,0.333333333333333,0.324975970727275,0.333333333333333,
0.324975970727275,0.333333333333333,0.324975970727275,0.333333333333333,
0.324975970727275,0.333333333333333,0.324975970727275,0.333333333333333,
0.324975970727275,0.333333333333333,0.324975970727275,0.333333333333333,
0.324975970727275,0.333333333333333,0.324975970727275,0.333333333333333,
0.324975970727275,0.333333333333333,0.324975970727275,0.333333333333333,
0.324975970727275,0.333333333333333,0.324975970727275,0.333333333333333,
0.324975970727275,0.333333333333333,0.324975970727275,0.333333333333333,
0.324975970727275,0.333333333333333,0.324975970727275,0.333333333333333,
0.324975970727275,0.333333333333333,0.324975970727275,0.333333333333333,
0.324975970727275,0.333333333333333),(1.,0.974927912181824,1.,0.974927912181824,
1.,0.974927912181824,1.,0.974927912181824,1.,0.974927912181824,1.,0.974927912181824,
1.,0.974927912181824,1.,0.974927912181824,1.,0.974927912181824,1.,0.974927912181824,
1.,0.974927912181824,1.,0.974927912181824,1.,0.974927912181824,1.,0.974927912181824,
1.,0.974927912181824,1.,0.974927912181824,1.,0.974927912181824,1.,0.974927912181824,
1.,0.974927912181824,1.,0.974927912181824,1.,0.974927912181824,1.,0.974927912181824,
1.,0.974927912181824,1.,0.974927912181824,1.,0.974927912181824,1.,0.974927912181824,
1.,0.974927912181824,1.,0.974927912181824,1.,0.974927912181824,1.,0.974927912181824,
1.,0.974927912181824,1.,0.974927912181824,1.,0.974927912181824,1.,0.974927912181824,
1.,0.974927912181824,1.,0.974927912181824,1.,0.974927912181824,1.,0.974927912181824,
1.,0.974927912181824,1.,0.974927912181824,1.,0.974927912181824,1.,0.974927912181824,
1.,0.974927912181824,1.,0.974927912181824,1.,0.974927912181824,1.,0.974927912181824,
1.,0.974927912181824,1.,0.974927912181824,1.,0.974927912181824,1.,0.974927912181824,
1.,0.974927912181824,1.,0.974927912181824,1.,0.974927912181824,1.,0.974927912181824,
1.,0.974927912181824,1.,0.974927912181824,1.,0.974927912181824,1.,0.974927912181824,
1.,0.974927912181824,1.,0.974927912181824,1.,0.974927912181824,1.,0.974927912181824,
1.,0.974927912181824,1.,0.974927912181824,1.,0.974927912181824,1.,0.974927912181824,
1.,0.974927912181824,1.,0.974927912181824,1.,0.974927912181824,1.,0.974927912181824,
1.)))
REPRESENTATION_ITEM('')
SURFACE()
);
#37=B_SPLINE_CURVE_WITH_KNOTS('',3,(#4016,#4017,#4018,#4019,#4020,#4021,
#4022,#4023,#4024,#4025,#4026,#4027,#4028,#4029,#4030,#4031,#4032,#4033,
#4034,#4035,#4036,#4037,#4038,#4039,#4040,#4041,#4042,#4043,#4044,#4045,
#4046,#4047,#4048,#4049,#4050,#4051,#4052,#4053,#4054,#4055,#4056,#4057,
#4058,#4059,#4060,#4061,#4062,#4063,#4064,#4065,#4066,#4067,#4068,#4069,
#4070,#4071,#4072,#4073,#4074,#4075,#4076,#4077,#4078,#4079,#4080,#4081,
#4082,#4083,#4084,#4085,#4086,#4087,#4088,#4089,#4090,#4091,#4092,#4093,
#4094,#4095,#4096,#4097,#4098,#4099,#4100,#4101,#4102,#4103,#4104,#4105,
#4106,#4107,#4108,#4109,#4110,#4111,#4112,#4113,#4114,#4115,#4116,#4117,
#4118,#4119,#4120,#4121,#4122,#4123,#4124,#4125,#4126,#4127,#4128,#4129,
#4130,#4131,#4132,#4133,#4134,#4135,#4136,#4137,#4138,#4139,#4140,#4141,
#4142,#4143,#4144,#4145,#4146,#4147,#4148,#4149,#4150,#4151,#4152,#4153,
#4154,#4155,#4156,#4157,#4158,#4159,#4160,#4161,#4162,#4163,#4164,#4165,
#4166,#4167,#4168,#4169,#4170,#4171,#4172,#4173,#4174,#4175,#4176,#4177,
#4178,#4179,#4180,#4181,#4182,#4183,#4184,#4185,#4186,#4187,#4188,#4189,
#4190,#4191,#4192,#4193,#4194,#4195,#4196,#4197,#4198,#4199,#4200,#4201,
#4202,#4203,#4204,#4205,#4206,#4207,#4208,#4209,#4210,#4211,#4212,#4213,
#4214,#4215,#4216,#4217,#4218,#4219,#4220,#4221,#4222,#4223,#4224,#4225,
#4226,#4227,#4228,#4229,#4230,#4231,#4232,#4233,#4234,#4235,#4236,#4237,
#4238,#4239,#4240,#4241),.UNSPECIFIED.,.F.,.F.,(4,3,3,3,3,3,3,3,3,3,3,3,
3,3,3,3,3,3,3,3,3,3,3,3,3,3,3,3,3,3,3,3,3,3,3,3,3,3,3,3,3,3,3,3,3,3,3,3,
3,3,3,3,3,3,3,3,3,3,3,3,3,3,3,3,3,3,3,3,3,3,3,3,3,3,3,4),(0.505622875727277,
0.517988160946919,0.520338789948538,0.520905429501515,0.52717265317845,
0.533305555196153,0.535054704170684,0.537132103408132,0.54490516587315,
0.552830838419486,0.563272810879374,0.564486532614977,0.568546357321302,
0.584201801943347,0.599912293797433,0.607745612443856,0.615542041404178,
0.623350189503564,0.631056029515969,0.6456920985192,0.646842539795389,0.661283412185915,
0.66268246093576,0.677297370184217,0.67824270230549,0.682213846392151,0.691716213252626,
0.693762976426177,0.703275083336273,0.709570647326886,0.711645674836442,
0.720271652950763,0.725345909407201,0.734085257246458,0.741077503280732,
0.741106647260554,0.748435460391805,0.751860029569614,0.755793417502878,
0.757713958294146,0.76570174867477,0.770509331725024,0.773347178256837,
0.779737634087422,0.785225245947169,0.785728872145709,0.794897633981219,
0.799848096300002,0.799941160169314,0.807299117280385,0.81097809583592,
0.814316370179752,0.814657074391455,0.818043484932961,0.829372988613599,
0.833425179548027,0.83673094572467,0.840594242287955,0.844088902835742,
0.849462701918626,0.858804817057886,0.864830932205664,0.880572108534982,
0.896355862867048,0.912005776159084,0.917668473946477,0.927580474989763,
0.938300332984732,0.943299451007609,0.947100302390772,0.958694413066092,
0.961816216612921,0.969174173723996,0.972967833922422,0.974936906461323,
0.97653213083507),.UNSPECIFIED.);
#38=B_SPLINE_CURVE_WITH_KNOTS('',3,(#4245,#4246,#4247,#4248,#4249,#4250,
#4251,#4252,#4253,#4254,#4255,#4256,#4257,#4258,#4259,#4260,#4261,#4262,
#4263,#4264),.UNSPECIFIED.,.F.,.F.,(4,2,2,2,2,2,2,2,2,4),(0.,0.0116792314509369,
0.023969165868339,0.036250854130431,0.050588906263982,0.0651100872670082,
0.0773226289799043,0.089228359128315,0.0957523155277064,0.102264320227649),
 .UNSPECIFIED.);
#39=B_SPLINE_CURVE_WITH_KNOTS('',3,(#5257,#5258,#5259,#5260,#5261,#5262,
#5263,#5264,#5265,#5266,#5267,#5268,#5269,#5270,#5271,#5272,#5273,#5274,
#5275,#5276,#5277,#5278,#5279,#5280),.UNSPECIFIED.,.F.,.F.,(4,2,2,2,2,2,
2,2,2,2,2,4),(9.99991793790667E-7,0.0409954758355881,0.116426326291497,
0.178802457956817,0.201487661798833,0.216832635254426,0.230582029229575,
0.246869198666259,0.271413998785539,0.302825983747229,0.319030712132421,
0.33517722448993),.UNSPECIFIED.);
#40=B_SPLINE_CURVE_WITH_KNOTS('',3,(#5282,#5283,#5284,#5285,#5286,#5287,
#5288,#5289,#5290,#5291,#5292,#5293,#5294,#5295,#5296,#5297,#5298,#5299,
#5300,#5301,#5302,#5303,#5304,#5305,#5306,#5307,#5308,#5309,#5310,#5311,
#5312,#5313,#5314,#5315,#5316,#5317,#5318,#5319,#5320,#5321,#5322,#5323,
#5324,#5325,#5326,#5327,#5328,#5329,#5330,#5331,#5332,#5333,#5334,#5335,
#5336,#5337,#5338,#5339,#5340,#5341,#5342,#5343,#5344,#5345,#5346,#5347,
#5348,#5349,#5350,#5351,#5352,#5353,#5354,#5355,#5356,#5357,#5358,#5359,
#5360,#5361,#5362,#5363,#5364,#5365,#5366,#5367,#5368,#5369,#5370,#5371,
#5372,#5373,#5374,#5375,#5376,#5377,#5378,#5379,#5380,#5381,#5382,#5383,
#5384,#5385,#5386,#5387,#5388,#5389,#5390,#5391,#5392,#5393,#5394,#5395,
#5396,#5397,#5398,#5399,#5400,#5401,#5402,#5403,#5404,#5405,#5406,#5407,
#5408,#5409,#5410,#5411,#5412,#5413,#5414,#5415,#5416,#5417,#5418,#5419,
#5420,#5421,#5422,#5423,#5424,#5425,#5426,#5427,#5428,#5429,#5430,#5431,
#5432,#5433,#5434,#5435,#5436,#5437,#5438,#5439,#5440,#5441,#5442,#5443,
#5444,#5445,#5446,#5447,#5448,#5449,#5450,#5451,#5452,#5453,#5454,#5455,
#5456,#5457,#5458,#5459,#5460,#5461,#5462,#5463,#5464,#5465,#5466,#5467,
#5468,#5469,#5470,#5471,#5472,#5473,#5474,#5475,#5476,#5477,#5478,#5479,
#5480,#5481,#5482,#5483,#5484,#5485,#5486,#5487,#5488,#5489,#5490,#5491,
#5492,#5493,#5494,#5495,#5496,#5497,#5498,#5499,#5500,#5501,#5502,#5503,
#5504,#5505,#5506,#5507,#5508,#5509,#5510,#5511,#5512,#5513,#5514,#5515,
#5516,#5517,#5518,#5519,#5520,#5521,#5522,#5523,#5524,#5525,#5526,#5527,
#5528,#5529,#5530,#5531,#5532,#5533,#5534,#5535,#5536,#5537,#5538,#5539,
#5540,#5541,#5542,#5543,#5544,#5545,#5546,#5547,#5548,#5549,#5550,#5551,
#5552,#5553,#5554,#5555,#5556,#5557,#5558,#5559,#5560,#5561,#5562,#5563,
#5564,#5565,#5566,#5567,#5568,#5569,#5570,#5571,#5572,#5573,#5574,#5575,
#5576,#5577,#5578,#5579,#5580,#5581,#5582,#5583,#5584,#5585,#5586,#5587,
#5588,#5589,#5590,#5591,#5592,#5593,#5594,#5595,#5596,#5597,#5598,#5599,
#5600,#5601,#5602,#5603,#5604,#5605,#5606,#5607,#5608,#5609,#5610,#5611,
#5612,#5613,#5614,#5615,#5616,#5617,#5618,#5619,#5620,#5621,#5622,#5623,
#5624,#5625,#5626,#5627,#5628,#5629,#5630,#5631,#5632,#5633,#5634,#5635,
#5636,#5637,#5638,#5639,#5640,#5641,#5642,#5643,#5644,#5645,#5646,#5647,
#5648,#5649,#5650,#5651,#5652,#5653,#5654,#5655,#5656,#5657,#5658,#5659,
#5660,#5661,#5662,#5663,#5664,#5665,#5666,#5667,#5668,#5669,#5670,#5671,
#5672,#5673,#5674,#5675,#5676,#5677,#5678,#5679,#5680,#5681,#5682,#5683,
#5684,#5685,#5686,#5687,#5688,#5689,#5690,#5691,#5692,#5693,#5694,#5695,
#5696,#5697,#5698,#5699,#5700,#5701,#5702,#5703,#5704,#5705,#5706,#5707,
#5708,#5709,#5710,#5711,#5712,#5713,#5714,#5715,#5716,#5717,#5718,#5719,
#5720,#5721,#5722,#5723,#5724,#5725,#5726,#5727,#5728,#5729,#5730,#5731,
#5732,#5733,#5734,#5735,#5736,#5737,#5738,#5739,#5740,#5741,#5742,#5743,
#5744,#5745,#5746,#5747,#5748,#5749,#5750,#5751,#5752,#5753,#5754,#5755,
#5756,#5757,#5758,#5759,#5760,#5761,#5762,#5763,#5764,#5765,#5766,#5767,
#5768,#5769,#5770,#5771,#5772,#5773,#5774,#5775,#5776,#5777,#5778,#5779,
#5780,#5781,#5782,#5783,#5784,#5785,#5786,#5787,#5788,#5789,#5790,#5791,
#5792,#5793,#5794,#5795,#5796,#5797,#5798,#5799,#5800,#5801,#5802,#5803,
#5804,#5805,#5806,#5807,#5808,#5809,#5810,#5811,#5812,#5813,#5814,#5815,
#5816,#5817,#5818,#5819,#5820,#5821,#5822,#5823,#5824,#5825,#5826,#5827,
#5828,#5829,#5830,#5831,#5832,#5833,#5834,#5835,#5836,#5837,#5838,#5839,
#5840,#5841,#5842,#5843,#5844,#5845,#5846,#5847,#5848,#5849,#5850,#5851,
#5852,#5853,#5854,#5855,#5856,#5857,#5858,#5859,#5860,#5861,#5862,#5863,
#5864,#5865,#5866,#5867,#5868,#5869,#5870,#5871,#5872,#5873,#5874,#5875,
#5876,#5877,#5878,#5879,#5880,#5881,#5882,#5883,#5884,#5885,#5886,#5887,
#5888,#5889,#5890,#5891,#5892,#5893,#5894,#5895,#5896,#5897,#5898,#5899,
#5900,#5901,#5902,#5903,#5904,#5905,#5906,#5907,#5908,#5909,#5910,#5911,
#5912,#5913,#5914,#5915,#5916,#5917,#5918,#5919,#5920,#5921,#5922,#5923,
#5924,#5925,#5926,#5927,#5928,#5929,#5930,#5931,#5932,#5933,#5934,#5935,
#5936,#5937,#5938,#5939,#5940,#5941,#5942,#5943,#5944,#5945,#5946,#5947,
#5948,#5949,#5950,#5951,#5952,#5953,#5954,#5955,#5956,#5957,#5958,#5959,
#5960,#5961,#5962,#5963,#5964,#5965,#5966,#5967,#5968,#5969,#5970,#5971,
#5972,#5973,#5974,#5975,#5976,#5977,#5978,#5979,#5980,#5981,#5982,#5983,
#5984,#5985,#5986,#5987,#5988,#5989,#5990,#5991,#5992,#5993,#5994,#5995,
#5996,#5997,#5998,#5999,#6000,#6001,#6002,#6003,#6004,#6005,#6006,#6007,
#6008,#6009,#6010,#6011,#6012,#6013,#6014,#6015,#6016,#6017,#6018,#6019,
#6020,#6021,#6022,#6023,#6024,#6025,#6026,#6027,#6028,#6029,#6030,#6031,
#6032,#6033,#6034,#6035,#6036,#6037,#6038,#6039,#6040,#6041,#6042,#6043,
#6044,#6045,#6046,#6047,#6048,#6049,#6050,#6051,#6052,#6053,#6054,#6055,
#6056,#6057,#6058,#6059,#6060,#6061,#6062,#6063,#6064,#6065,#6066,#6067,
#6068,#6069,#6070,#6071,#6072,#6073,#6074,#6075,#6076,#6077,#6078,#6079,
#6080,#6081,#6082,#6083,#6084,#6085,#6086,#6087,#6088,#6089,#6090,#6091,
#6092,#6093,#6094,#6095,#6096,#6097,#6098,#6099,#6100,#6101,#6102,#6103,
#6104,#6105,#6106,#6107,#6108,#6109,#6110,#6111,#6112,#6113,#6114,#6115,
#6116,#6117,#6118,#6119,#6120,#6121,#6122,#6123,#6124,#6125,#6126,#6127,
#6128,#6129,#6130,#6131,#6132,#6133,#6134,#6135,#6136,#6137,#6138,#6139,
#6140,#6141,#6142,#6143,#6144,#6145,#6146,#6147,#6148,#6149,#6150,#6151,
#6152,#6153,#6154,#6155,#6156,#6157,#6158,#6159,#6160,#6161,#6162,#6163,
#6164,#6165,#6166,#6167,#6168,#6169,#6170,#6171,#6172,#6173,#6174,#6175,
#6176,#6177,#6178,#6179,#6180,#6181,#6182,#6183,#6184,#6185,#6186,#6187,
#6188,#6189,#6190,#6191,#6192,#6193,#6194,#6195,#6196,#6197,#6198,#6199,
#6200,#6201,#6202,#6203,#6204,#6205,#6206,#6207,#6208,#6209,#6210,#6211,
#6212,#6213,#6214,#6215,#6216,#6217,#6218,#6219,#6220,#6221,#6222,#6223,
#6224,#6225,#6226,#6227,#6228,#6229,#6230,#6231,#6232,#6233,#6234,#6235,
#6236,#6237,#6238,#6239,#6240,#6241,#6242,#6243,#6244,#6245,#6246,#6247,
#6248,#6249,#6250,#6251,#6252,#6253,#6254,#6255,#6256,#6257,#6258,#6259,
#6260,#6261,#6262,#6263,#6264,#6265,#6266,#6267,#6268,#6269,#6270,#6271,
#6272,#6273,#6274,#6275,#6276,#6277,#6278,#6279,#6280,#6281,#6282,#6283,
#6284,#6285,#6286,#6287,#6288,#6289,#6290,#6291,#6292,#6293,#6294,#6295,
#6296,#6297,#6298,#6299,#6300,#6301,#6302,#6303,#6304,#6305,#6306,#6307,
#6308,#6309,#6310,#6311,#6312,#6313,#6314,#6315,#6316,#6317,#6318,#6319,
#6320,#6321,#6322,#6323,#6324,#6325,#6326,#6327,#6328,#6329,#6330,#6331,
#6332,#6333,#6334,#6335,#6336,#6337,#6338,#6339,#6340,#6341,#6342,#6343,
#6344,#6345,#6346,#6347,#6348,#6349,#6350,#6351,#6352,#6353,#6354,#6355,
#6356,#6357,#6358,#6359,#6360,#6361,#6362,#6363,#6364,#6365,#6366,#6367,
#6368,#6369,#6370,#6371,#6372,#6373,#6374,#6375,#6376,#6377,#6378,#6379,
#6380,#6381,#6382,#6383,#6384,#6385,#6386,#6387,#6388,#6389,#6390,#6391,
#6392,#6393,#6394,#6395,#6396,#6397,#6398,#6399,#6400,#6401,#6402,#6403,
#6404,#6405,#6406,#6407,#6408,#6409,#6410,#6411,#6412,#6413,#6414,#6415,
#6416,#6417,#6418,#6419,#6420,#6421,#6422,#6423,#6424,#6425,#6426,#6427,
#6428,#6429,#6430,#6431,#6432,#6433,#6434,#6435,#6436,#6437,#6438,#6439,
#6440,#6441,#6442,#6443,#6444,#6445,#6446,#6447,#6448,#6449,#6450,#6451,
#6452,#6453,#6454,#6455,#6456,#6457,#6458,#6459,#6460,#6461,#6462,#6463,
#6464,#6465,#6466,#6467,#6468,#6469,#6470,#6471,#6472,#6473,#6474,#6475,
#6476),.UNSPECIFIED.,.F.,.F.,(4,3,3,3,3,3,3,3,3,3,3,3,3,3,3,3,3,3,3,3,3,
3,3,3,3,3,3,3,3,3,3,3,3,3,3,3,3,3,3,3,3,3,3,3,3,3,3,3,3,3,3,3,3,3,3,3,3,
3,3,3,3,3,3,3,3,3,3,3,3,3,3,3,3,3,3,3,3,3,3,3,3,3,3,3,3,3,3,3,3,3,3,3,3,
3,3,3,3,3,3,3,3,3,3,3,3,3,3,3,3,3,3,3,3,3,3,3,3,3,3,3,3,3,3,3,3,3,3,3,3,
3,3,3,3,3,3,3,3,3,3,3,3,3,3,3,3,3,3,3,3,3,3,3,3,3,3,3,3,3,3,3,3,3,3,3,3,
3,3,3,3,3,3,3,3,3,3,3,3,3,3,3,3,3,3,3,3,3,3,3,3,3,3,3,3,3,3,3,3,3,3,3,3,
3,3,3,3,3,3,3,3,3,3,3,3,3,3,3,3,3,3,3,3,3,3,3,3,3,3,3,3,3,3,3,3,3,3,3,3,
3,3,3,3,3,3,3,3,3,3,3,3,3,3,3,3,3,3,3,3,3,3,3,3,3,3,3,3,3,3,3,3,3,3,3,3,
3,3,3,3,3,3,3,3,3,3,3,3,3,3,3,3,3,3,3,3,3,3,3,3,3,3,3,3,3,3,3,3,3,3,3,3,
3,3,3,3,3,3,3,3,3,3,3,3,3,3,3,3,3,3,3,3,3,3,3,3,3,3,3,3,3,3,3,3,3,3,3,3,
3,3,3,3,3,3,3,3,3,3,3,3,3,3,3,3,3,3,3,3,3,3,3,3,3,3,3,3,3,3,3,3,3,3,3,3,
3,3,3,3,3,3,3,3,3,3,3,3,3,3,3,3,3,4),(0.0434521468850362,0.0461873441657508,
0.0489269991702234,0.0516650038763463,0.0544039305096017,0.0571428571428571,
0.059877893422679,0.0626138848522894,0.065352304603236,0.0680886385499103,
0.0708234140605492,0.0714285714285714,0.0741636077083921,0.0768995991380027,
0.0796380188889482,0.0823743528356205,0.0851091283462598,0.0857142857142857,
0.0884493219941073,0.0911853134237064,0.093923733174652,0.0966600671213259,
0.0993948426319571,0.1,0.102735036279824,0.105471027709443,0.108209447460392,
0.110945781407079,0.113680556917732,0.114285714285714,0.117020750565535,
0.119756741995136,0.122495161746079,0.125231495692751,0.127966271203388,
0.128571428571429,0.131306464851251,0.134042456280861,0.136780876031805,
0.139517209978476,0.142251985489111,0.142857142857143,0.145592179136964,
0.148328170566579,0.151066590317524,0.153802924264195,0.156537699774842,
0.157142857142857,0.159877893422678,0.162613884852275,0.165352304603217,
0.168088638549894,0.170823414060526,0.171428571428571,0.174163607708387,
0.176899599137999,0.179638018888945,0.182374352835622,0.185109128346255,
0.185714285714286,0.188449321994121,0.191185313423734,0.193923733174678,
0.196660067121338,0.199394842631953,0.2,0.202735036279828,0.205471027709437,
0.208209447460376,0.210945781407047,0.21368055691771,0.214285714285714,
0.217020750565534,0.21975674199515,0.222495161746102,0.225231495692787,
0.227966271203424,0.228571428571429,0.231306464851263,0.23404245628089,
0.236780876031837,0.239517209978489,0.242251985489098,0.242857142857143,
0.245592179136972,0.248328170566582,0.251066590317521,0.253802924264199,
0.256537699774829,0.257142857142857,0.259877893422686,0.26261388485229,
0.265352304603237,0.268088638549896,0.270823414060528,0.271428571428571,
0.2741636077084,0.276899599138014,0.27963801888896,0.282374352835653,0.285109128346286,
0.285714285714286,0.28844932199411,0.291185313423707,0.293923733174651,
0.296660067121322,0.299394842631966,0.3,0.302735036279835,0.305471027709446,
0.308209447460395,0.310945781407089,0.313680556917723,0.314285714285714,
0.31702075056553,0.319756741995162,0.322495161746109,0.325231495692777,
0.32796627120343,0.328571428571429,0.331306464851255,0.334042456280855,
0.336780876031804,0.339517209978488,0.342251985489124,0.342857142857143,
0.345592179136954,0.348328170566521,0.351066590317465,0.353802924264142,
0.3565376997748,0.357142857142857,0.359877893422679,0.362613884852294,0.365352304603241,
0.368088638549919,0.370823414060555,0.371428571428571,0.374163607708382,
0.376899599137964,0.37963801888891,0.382374352835591,0.385109128346204,
0.385714285714286,0.388449321994103,0.391185313423703,0.393923733174653,
0.396660067121351,0.399394842632005,0.4,0.402735036279825,0.405471027709447,
0.408209447460393,0.410945781407081,0.413680556917718,0.414285714285714,
0.417020750565532,0.419756741995165,0.422495161746111,0.425231495692786,
0.427966271203415,0.428571428571429,0.431306464851253,0.434042456280863,
0.436780876031811,0.439517209978483,0.442251985489122,0.442857142857143,
0.445592179136974,0.448328170566577,0.451066590317522,0.453802924264206,
0.45653769977484,0.457142857142857,0.459877893422679,0.462613884852274,
0.46535230460322,0.468088638549892,0.470823414060526,0.471428571428571,
0.474163607708389,0.476899599137977,0.479638018888923,0.482374352835603,
0.485109128346238,0.485714285714286,0.488449321994099,0.491185313423694,
0.493923733174635,0.496660067121315,0.499394842631956,0.5,0.502735036279827,
0.505471027709436,0.508209447460376,0.510945781407021,0.513680556917665,
0.514285714285714,0.517020750565532,0.519756741995121,0.522495161746054,
0.525231495692741,0.527966271203371,0.528571428571429,0.531306464851231,
0.534042456280826,0.53678087603177,0.539517209978444,0.542251985489095,
0.542857142857143,0.545592179136964,0.54832817056658,0.551066590317522,
0.553802924264182,0.556537699774845,0.557142857142857,0.559877893422674,
0.562613884852282,0.565352304603234,0.568088638549889,0.570823414060542,
0.571428571428571,0.574163607708401,0.576899599138019,0.579638018888965,
0.582374352835606,0.585109128346239,0.585714285714286,0.588449321994126,
0.591185313423754,0.5939237331747,0.596660067121342,0.599394842631994,0.6,
0.60273503627982,0.605471027709411,0.608209447460348,0.610945781407044,
0.613680556917701,0.614285714285714,0.617020750565514,0.619756741995111,
0.622495161746057,0.625231495692732,0.627966271203357,0.628571428571429,
0.631306464851258,0.634042456280886,0.636780876031825,0.639517209978507,
0.642251985489135,0.642857142857143,0.645592179136954,0.648328170566526,
0.651066590317477,0.653802924264148,0.656537699774774,0.657142857142857,
0.65987789342268,0.662613884852296,0.66535230460324,0.668088638549891,0.670823414060543,
0.671428571428571,0.674163607708392,0.676899599138033,0.679638018888974,
0.682374352835659,0.685109128346312,0.685714285714286,0.688449321994104,
0.6911853134237,0.693923733174643,0.696660067121325,0.699394842631902,0.7,
0.702735036279801,0.705471027709409,0.708209447460343,0.710945781407061,
0.713680556917779,0.714285714285714,0.717020750565534,0.719756741995116,
0.722495161746074,0.72523149569276,0.727966271203408,0.728571428571429,
0.731306464851277,0.734042456280897,0.736780876031841,0.739517209978497,
0.742251985489142,0.742857142857143,0.745592179136962,0.748328170566599,
0.751066590317548,0.753802924264176,0.756537699774778,0.757142857142857,
0.759877893422655,0.762613884852237,0.765352304603176,0.768088638549865,
0.770823414060485,0.771428571428571,0.774163607708391,0.776899599137959,
0.77963801888891,0.782374352835568,0.785109128346213,0.785714285714286,
0.788449321994106,0.791185313423719,0.793923733174654,0.796660067121301,
0.799394842631947,0.8,0.802735036279805,0.805471027709432,0.808209447460388,
0.810945781407092,0.813680556917737,0.814285714285714,0.817020750565548,
0.819756741995165,0.822495161746102,0.825231495692781,0.827966271203429,
0.828571428571429,0.831306464851221,0.83404245628079,0.836780876031735,
0.8395172099784,0.842251985489027,0.842857142857143,0.845592179136976,0.84832817056658,
0.851066590317534,0.853802924264192,0.856537699774856,0.857142857142857,
0.85987789342267,0.86261388485227,0.865352304603208,0.868088638549884,0.870823414060506,
0.871428571428571,0.874163607708391,0.876899599137982,0.87963801888893,
0.882374352835648,0.88510912834627,0.885714285714286,0.888449321994109,
0.891185313423738,0.893923733174676,0.896660067121346,0.899394842631965,
0.9,0.902735036279826,0.9054710277094,0.908209447460347,0.910945781407016,
0.913680556917645,0.914285714285714,0.917020750565528,0.919756741995146,
0.922495161746083,0.925231495692764,0.927966271203396,0.928571428571429,
0.931306464851252,0.934042456280889,0.936780876031843,0.939517209978495,
0.942251985489148,0.942857142857143,0.945592179136907,0.948328170566525,
0.951066590317466,0.953802924264139,0.956537699774797,0.957142857142857,
0.95987789342267,0.962613884852283,0.965352304603234,0.968088638549892,
0.970823414060527,0.971428571428571,0.974163607708378,0.976899599137948,
0.979638018888884,0.982374352835551,0.985109128346214,0.985714285714286,
0.988448991390083,0.991186079127076,0.992296011182497),.UNSPECIFIED.);
#41=B_SPLINE_CURVE_WITH_KNOTS('',3,(#6478,#6479,#6480,#6481,#6482,#6483,
#6484,#6485,#6486,#6487,#6488,#6489,#6490,#6491,#6492,#6493,#6494,#6495,
#6496,#6497,#6498,#6499,#6500,#6501,#6502,#6503,#6504,#6505,#6506,#6507,
#6508,#6509,#6510,#6511,#6512,#6513,#6514,#6515,#6516,#6517,#6518,#6519,
#6520,#6521,#6522,#6523,#6524,#6525,#6526,#6527,#6528,#6529,#6530,#6531,
#6532,#6533,#6534,#6535,#6536,#6537,#6538,#6539,#6540,#6541,#6542,#6543,
#6544,#6545,#6546,#6547,#6548,#6549,#6550,#6551,#6552,#6553,#6554,#6555,
#6556,#6557,#6558,#6559,#6560,#6561,#6562,#6563,#6564,#6565,#6566,#6567,
#6568,#6569,#6570,#6571,#6572,#6573,#6574,#6575,#6576,#6577,#6578,#6579,
#6580,#6581,#6582,#6583,#6584,#6585,#6586,#6587,#6588,#6589,#6590,#6591,
#6592,#6593,#6594,#6595,#6596,#6597,#6598,#6599,#6600,#6601,#6602,#6603,
#6604,#6605,#6606,#6607,#6608,#6609,#6610,#6611,#6612,#6613,#6614,#6615,
#6616,#6617,#6618,#6619,#6620,#6621,#6622,#6623,#6624,#6625,#6626,#6627,
#6628,#6629,#6630,#6631,#6632,#6633,#6634,#6635,#6636,#6637,#6638,#6639,
#6640,#6641,#6642,#6643,#6644,#6645,#6646,#6647,#6648,#6649,#6650,#6651,
#6652,#6653,#6654,#6655,#6656,#6657,#6658,#6659,#6660,#6661,#6662,#6663,
#6664,#6665,#6666,#6667,#6668,#6669,#6670,#6671,#6672,#6673,#6674,#6675,
#6676,#6677,#6678,#6679,#6680,#6681,#6682,#6683,#6684,#6685,#6686,#6687,
#6688,#6689,#6690,#6691,#6692,#6693,#6694,#6695,#6696,#6697,#6698,#6699,
#6700,#6701,#6702,#6703,#6704,#6705,#6706,#6707,#6708,#6709,#6710,#6711,
#6712,#6713,#6714,#6715,#6716,#6717,#6718,#6719,#6720,#6721,#6722,#6723,
#6724,#6725,#6726,#6727,#6728,#6729,#6730,#6731,#6732,#6733,#6734,#6735,
#6736,#6737,#6738,#6739,#6740,#6741,#6742,#6743,#6744,#6745,#6746,#6747,
#6748,#6749,#6750,#6751,#6752,#6753,#6754,#6755,#6756,#6757,#6758,#6759,
#6760,#6761,#6762,#6763,#6764,#6765,#6766,#6767,#6768,#6769,#6770,#6771,
#6772,#6773,#6774,#6775,#6776,#6777,#6778,#6779,#6780,#6781,#6782,#6783,
#6784,#6785,#6786,#6787,#6788,#6789,#6790,#6791,#6792,#6793,#6794,#6795,
#6796,#6797,#6798,#6799,#6800,#6801,#6802,#6803,#6804,#6805,#6806,#6807,
#6808,#6809,#6810,#6811,#6812,#6813,#6814,#6815,#6816,#6817,#6818,#6819,
#6820,#6821,#6822,#6823,#6824,#6825,#6826,#6827,#6828,#6829,#6830,#6831,
#6832,#6833,#6834,#6835,#6836,#6837,#6838,#6839,#6840,#6841,#6842,#6843,
#6844,#6845,#6846,#6847,#6848,#6849,#6850,#6851,#6852,#6853,#6854,#6855,
#6856,#6857,#6858,#6859,#6860,#6861,#6862,#6863,#6864,#6865,#6866,#6867,
#6868,#6869,#6870,#6871,#6872,#6873,#6874,#6875,#6876,#6877,#6878,#6879,
#6880,#6881,#6882,#6883,#6884,#6885,#6886,#6887,#6888,#6889,#6890,#6891,
#6892,#6893,#6894,#6895,#6896,#6897,#6898,#6899,#6900,#6901,#6902,#6903,
#6904,#6905,#6906,#6907,#6908,#6909,#6910,#6911,#6912,#6913,#6914,#6915,
#6916,#6917,#6918,#6919,#6920,#6921,#6922,#6923,#6924,#6925,#6926,#6927,
#6928,#6929,#6930,#6931,#6932,#6933,#6934,#6935,#6936,#6937,#6938,#6939,
#6940,#6941,#6942,#6943,#6944,#6945,#6946,#6947,#6948,#6949,#6950,#6951,
#6952,#6953,#6954,#6955,#6956,#6957,#6958,#6959,#6960,#6961,#6962,#6963,
#6964,#6965,#6966,#6967,#6968,#6969,#6970,#6971,#6972,#6973,#6974,#6975,
#6976,#6977,#6978,#6979,#6980,#6981,#6982,#6983,#6984,#6985,#6986,#6987,
#6988,#6989,#6990,#6991,#6992,#6993,#6994,#6995,#6996,#6997,#6998,#6999,
#7000,#7001,#7002,#7003,#7004,#7005,#7006,#7007,#7008,#7009,#7010,#7011,
#7012,#7013,#7014,#7015,#7016,#7017,#7018,#7019,#7020,#7021,#7022,#7023,
#7024,#7025,#7026,#7027,#7028,#7029,#7030,#7031,#7032,#7033,#7034,#7035,
#7036,#7037,#7038,#7039,#7040,#7041,#7042,#7043,#7044,#7045,#7046,#7047,
#7048,#7049,#7050,#7051,#7052,#7053,#7054,#7055,#7056,#7057,#7058,#7059,
#7060,#7061,#7062,#7063,#7064,#7065,#7066,#7067,#7068,#7069,#7070,#7071,
#7072,#7073,#7074,#7075,#7076,#7077,#7078,#7079,#7080,#7081,#7082,#7083,
#7084,#7085,#7086,#7087,#7088,#7089,#7090,#7091,#7092,#7093,#7094,#7095,
#7096,#7097,#7098,#7099,#7100,#7101,#7102,#7103,#7104,#7105,#7106,#7107,
#7108,#7109,#7110,#7111,#7112,#7113,#7114,#7115,#7116,#7117,#7118,#7119,
#7120,#7121,#7122,#7123,#7124,#7125,#7126,#7127,#7128,#7129,#7130,#7131,
#7132,#7133,#7134,#7135,#7136,#7137,#7138,#7139,#7140,#7141,#7142,#7143,
#7144,#7145,#7146,#7147,#7148,#7149,#7150,#7151,#7152,#7153,#7154,#7155,
#7156,#7157,#7158,#7159,#7160,#7161,#7162,#7163,#7164,#7165,#7166,#7167,
#7168,#7169,#7170,#7171,#7172,#7173,#7174,#7175,#7176,#7177,#7178,#7179,
#7180,#7181,#7182,#7183,#7184,#7185,#7186,#7187,#7188,#7189,#7190,#7191,
#7192,#7193,#7194,#7195,#7196,#7197,#7198,#7199,#7200,#7201,#7202,#7203,
#7204,#7205,#7206,#7207,#7208,#7209,#7210,#7211,#7212,#7213,#7214,#7215,
#7216,#7217,#7218,#7219,#7220,#7221,#7222,#7223,#7224,#7225,#7226,#7227,
#7228,#7229,#7230,#7231,#7232,#7233,#7234,#7235,#7236,#7237,#7238,#7239,
#7240,#7241,#7242,#7243,#7244,#7245,#7246,#7247,#7248,#7249,#7250,#7251,
#7252,#7253,#7254,#7255,#7256,#7257,#7258,#7259,#7260,#7261,#7262,#7263,
#7264,#7265,#7266,#7267,#7268,#7269,#7270,#7271,#7272,#7273,#7274,#7275,
#7276,#7277,#7278,#7279,#7280,#7281,#7282,#7283,#7284,#7285,#7286,#7287,
#7288,#7289,#7290,#7291,#7292,#7293,#7294,#7295,#7296,#7297,#7298,#7299,
#7300,#7301,#7302,#7303,#7304,#7305,#7306,#7307,#7308,#7309,#7310,#7311,
#7312,#7313,#7314,#7315,#7316,#7317,#7318,#7319,#7320,#7321,#7322,#7323,
#7324,#7325,#7326,#7327,#7328,#7329,#7330,#7331,#7332,#7333,#7334,#7335,
#7336,#7337,#7338,#7339,#7340,#7341,#7342,#7343,#7344,#7345,#7346,#7347,
#7348,#7349,#7350,#7351,#7352,#7353,#7354,#7355,#7356,#7357,#7358,#7359,
#7360,#7361,#7362,#7363,#7364,#7365,#7366,#7367,#7368,#7369,#7370,#7371,
#7372,#7373,#7374,#7375,#7376,#7377,#7378,#7379,#7380,#7381,#7382,#7383,
#7384,#7385,#7386,#7387,#7388,#7389,#7390,#7391,#7392,#7393,#7394,#7395,
#7396,#7397,#7398,#7399,#7400,#7401,#7402,#7403,#7404,#7405,#7406,#7407,
#7408,#7409,#7410,#7411,#7412,#7413,#7414,#7415,#7416,#7417,#7418,#7419,
#7420,#7421,#7422,#7423,#7424,#7425,#7426,#7427,#7428,#7429,#7430,#7431,
#7432,#7433,#7434,#7435,#7436,#7437,#7438,#7439,#7440,#7441,#7442,#7443,
#7444,#7445,#7446,#7447,#7448,#7449,#7450,#7451,#7452,#7453,#7454,#7455,
#7456,#7457,#7458,#7459,#7460,#7461,#7462,#7463,#7464,#7465,#7466,#7467,
#7468,#7469,#7470,#7471,#7472,#7473,#7474,#7475,#7476,#7477,#7478,#7479,
#7480,#7481,#7482,#7483,#7484,#7485,#7486,#7487,#7488,#7489,#7490,#7491,
#7492,#7493,#7494,#7495,#7496,#7497,#7498,#7499,#7500,#7501,#7502,#7503,
#7504,#7505,#7506,#7507,#7508,#7509,#7510,#7511,#7512,#7513,#7514,#7515,
#7516,#7517,#7518,#7519,#7520,#7521,#7522,#7523,#7524,#7525,#7526,#7527,
#7528,#7529,#7530,#7531,#7532,#7533,#7534,#7535,#7536,#7537,#7538,#7539,
#7540,#7541,#7542,#7543,#7544,#7545,#7546,#7547,#7548,#7549,#7550,#7551,
#7552,#7553,#7554,#7555,#7556,#7557,#7558,#7559,#7560,#7561,#7562,#7563,
#7564,#7565,#7566,#7567,#7568,#7569,#7570,#7571,#7572,#7573,#7574,#7575,
#7576,#7577,#7578,#7579,#7580,#7581,#7582,#7583,#7584,#7585,#7586,#7587,
#7588,#7589,#7590,#7591,#7592,#7593,#7594,#7595,#7596,#7597,#7598,#7599,
#7600,#7601,#7602,#7603,#7604,#7605,#7606,#7607,#7608,#7609,#7610,#7611,
#7612,#7613,#7614,#7615,#7616,#7617,#7618,#7619,#7620,#7621,#7622,#7623,
#7624,#7625,#7626,#7627,#7628,#7629,#7630,#7631,#7632,#7633,#7634,#7635,
#7636,#7637,#7638,#7639,#7640,#7641,#7642,#7643,#7644,#7645,#7646,#7647,
#7648,#7649,#7650,#7651,#7652,#7653,#7654,#7655,#7656,#7657,#7658,#7659,
#7660,#7661,#7662,#7663,#7664,#7665,#7666,#7667,#7668,#7669,#7670,#7671,
#7672,#7673,#7674,#7675,#7676,#7677,#7678,#7679,#7680,#7681,#7682,#7683,
#7684,#7685,#7686,#7687,#7688,#7689,#7690,#7691,#7692,#7693,#7694,#7695,
#7696,#7697,#7698,#7699,#7700,#7701,#7702),.UNSPECIFIED.,.F.,.F.,(4,3,3,
3,3,3,3,3,3,3,3,3,3,3,3,3,3,3,3,3,3,3,3,3,3,3,3,3,3,3,3,3,3,3,3,3,3,3,3,
3,3,3,3,3,3,3,3,3,3,3,3,3,3,3,3,3,3,3,3,3,3,3,3,3,3,3,3,3,3,3,3,3,3,3,3,
3,3,3,3,3,3,3,3,3,3,3,3,3,3,3,3,3,3,3,3,3,3,3,3,3,3,3,3,3,3,3,3,3,3,3,3,
3,3,3,3,3,3,3,3,3,3,3,3,3,3,3,3,3,3,3,3,3,3,3,3,3,3,3,3,3,3,3,3,3,3,3,3,
3,3,3,3,3,3,3,3,3,3,3,3,3,3,3,3,3,3,3,3,3,3,3,3,3,3,3,3,3,3,3,3,3,3,3,3,
3,3,3,3,3,3,3,3,3,3,3,3,3,3,3,3,3,3,3,3,3,3,3,3,3,3,3,3,3,3,3,3,3,3,3,3,
3,3,3,3,3,3,3,3,3,3,3,3,3,3,3,3,3,3,3,3,3,3,3,3,3,3,3,3,3,3,3,3,3,3,3,3,
3,3,3,3,3,3,3,3,3,3,3,3,3,3,3,3,3,3,3,3,3,3,3,3,3,3,3,3,3,3,3,3,3,3,3,3,
3,3,3,3,3,3,3,3,3,3,3,3,3,3,3,3,3,3,3,3,3,3,3,3,3,3,3,3,3,3,3,3,3,3,3,3,
3,3,3,3,3,3,3,3,3,3,3,3,3,3,3,3,3,3,3,3,3,3,3,3,3,3,3,3,3,3,3,3,3,3,3,3,
3,3,3,3,3,3,3,3,3,3,3,3,3,3,3,3,3,3,3,3,3,3,3,3,3,3,3,3,3,3,3,3,3,3,3,3,
3,3,3,3,3,3,3,3,3,4),(0.023206495763431,0.0257239292490225,0.0282450189887502,
0.0285714285714286,0.0310923942810177,0.0336100262627011,0.0361278182416742,
0.0386450010909029,0.0411660098458559,0.0428571428571429,0.0453781085667337,
0.0478957405484203,0.0504135325273945,0.0529307153766255,0.0554517241315774,
0.0571428571428571,0.059663822852449,0.0621814548341318,0.0646992468131065,
0.0672164296623363,0.0697374384172902,0.0714285714285714,0.0739495371381627,
0.076467169119844,0.0789849610988178,0.0815021439480481,0.084023152703002,
0.0857142857142857,0.088235251423873,0.0907528834055563,0.0932706753845298,
0.0957878582337589,0.098308866988713,0.1,0.10252096570959,0.105038597691268,
0.107556389670243,0.110073572519475,0.112594581274429,0.114285714285714,
0.116806679995307,0.119324311976988,0.121842103955963,0.124359286805196,
0.126880295560147,0.128571428571429,0.131092394281013,0.133610026262683,
0.136127818241655,0.138645001090891,0.141166009845844,0.142857142857143,
0.145378108566732,0.147895740548422,0.150413532527396,0.152930715376634,
0.155451724131588,0.157142857142857,0.159663822852444,0.162181454834132,
0.164699246813105,0.167216429662338,0.169737438417291,0.171428571428571,
0.173949537138155,0.176467169119835,0.178984961098808,0.181502143948042,
0.184023152702995,0.185714285714286,0.188235251423882,0.190752883405569,
0.193270675384542,0.195787858233769,0.19830886698872,0.2,0.202520965709589,
0.205038597691277,0.207556389670251,0.210073572519482,0.212594581274431,
0.214285714285714,0.216806679995304,0.219324311976987,0.221842103955961,
0.224359286805185,0.226880295560131,0.228571428571429,0.231092394281016,
0.23361002626269,0.236127818241664,0.238645001090892,0.241166009845845,
0.242857142857143,0.245378108566735,0.247895740548416,0.25041353252739,
0.252930715376624,0.255451724131578,0.257142857142857,0.259663822852451,
0.262181454834138,0.264699246813112,0.267216429662339,0.269737438417293,
0.271428571428571,0.273949537138167,0.276467169119861,0.278984961098836,
0.281502143948073,0.284023152703024,0.285714285714286,0.288235251423881,
0.290752883405567,0.293270675384543,0.295787858233765,0.298308866988717,
0.3,0.302520965709596,0.30503859769128,0.307556389670252,0.31007357251948,
0.312594581274429,0.314285714285714,0.316806679995287,0.319324311976971,
0.321842103955943,0.324359286805174,0.326880295560125,0.328571428571429,
0.33109239428101,0.333610026262706,0.336127818241682,0.338645001090916,
0.34116600984586,0.342857142857143,0.345378108566721,0.347895740548409,
0.350413532527381,0.352930715376615,0.355451724131572,0.357142857142857,
0.359663822852443,0.362181454834099,0.364699246813074,0.367216429662306,
0.369737438417254,0.371428571428571,0.373949537138159,0.376467169119829,
0.378984961098804,0.381502143948016,0.384023152702971,0.385714285714286,
0.38823525142388,0.390752883405583,0.393270675384557,0.395787858233787,
0.398308866988739,0.4,0.402520965709584,0.405038597691256,0.407556389670229,
0.41007357251945,0.412594581274402,0.414285714285714,0.416806679995293,
0.419324311976974,0.421842103955951,0.424359286805177,0.426880295560129,
0.428571428571429,0.43109239428102,0.433610026262699,0.436127818241675,
0.438645001090902,0.441166009845859,0.442857142857143,0.445378108566734,
0.447895740548424,0.450413532527398,0.452930715376623,0.455451724131568,
0.457142857142857,0.459663822852451,0.462181454834118,0.464699246813092,
0.467216429662323,0.469737438417271,0.471428571428571,0.473949537138167,
0.476467169119847,0.478984961098823,0.481502143948057,0.484023152703002,
0.485714285714286,0.488235251423869,0.490752883405553,0.493270675384525,
0.495787858233748,0.498308866988705,0.5,0.502520965709591,0.505038597691261,
0.507556389670239,0.510073572519473,0.512594581274426,0.514285714285714,
0.516806679995304,0.519324311976992,0.521842103955964,0.524359286805211,
0.526880295560167,0.528571428571429,0.531092394281006,0.533610026262715,
0.53612781824169,0.538645001090917,0.541166009845867,0.542857142857143,
0.54537810856674,0.547895740548404,0.550413532527373,0.552930715376607,
0.555451724131568,0.557142857142857,0.559663822852453,0.562181454834126,
0.564699246813095,0.567216429662329,0.569737438417277,0.571428571428571,
0.57394953713816,0.576467169119855,0.578984961098832,0.581502143948056,
0.584023152703013,0.585714285714286,0.58823525142385,0.590752883405521,
0.593270675384497,0.595787858233757,0.598308866988711,0.6,0.602520965709609,
0.605038597691303,0.607556389670285,0.610073572519503,0.612594581274451,
0.614285714285714,0.616806679995288,0.619324311976971,0.621842103955946,
0.624359286805171,0.626880295560112,0.628571428571429,0.631092394281018,
0.633610026262711,0.636127818241686,0.638645001090888,0.641166009845846,
0.642857142857143,0.645378108566731,0.647895740548437,0.65041353252741,
0.652930715376643,0.655451724131588,0.657142857142857,0.659663822852448,
0.662181454834114,0.664699246813086,0.667216429662316,0.669737438417258,
0.671428571428571,0.673949537138158,0.67646716911984,0.67898496109881,0.681502143948056,
0.684023152703005,0.685714285714286,0.688235251423882,0.690752883405585,
0.693270675384566,0.695787858233805,0.698308866988762,0.7,0.7025209657096,
0.705038597691304,0.707556389670276,0.710073572519505,0.712594581274454,
0.714285714285714,0.716806679995296,0.719324311976947,0.721842103955917,
0.724359286805131,0.726880295560062,0.728571428571429,0.731092394281035,
0.733610026262732,0.736127818241713,0.738645001090942,0.741166009845897,
0.742857142857143,0.745378108566722,0.747895740548415,0.750413532527391,
0.752930715376615,0.75545172413156,0.757142857142857,0.759663822852465,
0.762181454834149,0.764699246813129,0.767216429662351,0.769737438417299,
0.771428571428571,0.773949537138153,0.776467169119842,0.778984961098804,
0.781502143948032,0.784023152702966,0.785714285714286,0.788235251423874,
0.790752883405565,0.793270675384545,0.795787858233779,0.79830886698873,
0.8,0.802520965709581,0.805038597691266,0.807556389670235,0.810073572519464,
0.812594581274417,0.814285714285714,0.816806679995304,0.819324311977038,
0.82184210395602,0.824359286805267,0.826880295560212,0.828571428571429,
0.831092394280992,0.833610026262696,0.836127818241669,0.838645001090894,
0.841166009845847,0.842857142857143,0.845378108566734,0.847895740548434,
0.850413532527405,0.852930715376647,0.855451724131588,0.857142857142857,
0.859663822852412,0.86218145483413,0.864699246813113,0.867216429662333,
0.869737438417301,0.871428571428571,0.873949537138163,0.876467169119875,
0.878984961098842,0.881502143948064,0.884023152703011,0.885714285714286,
0.888235251423884,0.890752883405557,0.893270675384532,0.895787858233751,
0.89830886698871,0.9,0.902520965709585,0.90503859769128,0.90755638967025,
0.910073572519495,0.912594581274447,0.914285714285714,0.916806679995308,
0.919324311977025,0.921842103956005,0.92435928680524,0.926880295560179,
0.928571428571429,0.931092394281023,0.933610026262707,0.936127818241673,
0.938645001090907,0.941166009845862,0.942857142857143,0.945378108566741,
0.947895740548478,0.950413532527452,0.952930715376688,0.955451724131655,
0.957142857142857,0.959663822852439,0.962181454834151,0.964699246813133,
0.967216429662383,0.969737438417352,0.971428571428572,0.973949537138156,
0.976467169119865,0.978984961098835,0.98150214394807,0.984023152703024,
0.985714285714286,0.988235247165933,0.990852917116709,0.993470587067484),
 .UNSPECIFIED.);
#42=B_SPLINE_CURVE_WITH_KNOTS('',3,(#7749,#7750,#7751,#7752,#7753,#7754,
#7755,#7756,#7757,#7758,#7759,#7760,#7761,#7762,#7763,#7764,#7765,#7766,
#7767,#7768,#7769,#7770,#7771,#7772),.UNSPECIFIED.,.F.,.F.,(4,2,2,2,2,2,
2,2,2,2,2,4),(9.99997522730752E-7,0.0373212594653978,0.0837444328860222,
0.127999538981999,0.168138172256258,0.195435295899977,0.213313281312765,
0.225803333956439,0.236147330446737,0.247437939130784,0.264210428398769,
0.300000948832372),.UNSPECIFIED.);
#43=B_SPLINE_CURVE_WITH_KNOTS('',3,(#7774,#7775,#7776,#7777,#7778,#7779,
#7780,#7781,#7782,#7783,#7784,#7785,#7786,#7787,#7788,#7789,#7790,#7791,
#7792,#7793),.UNSPECIFIED.,.F.,.F.,(4,2,2,2,2,2,2,2,2,4),(1.10999191885525E-10,
0.0114224997171007,0.0238925436228599,0.0362967112517097,0.0484706620322139,
0.0615854552568996,0.0761727562847049,0.0902646072806745,0.0975841853107938,
0.104919277808089),.UNSPECIFIED.);
#44=B_SPLINE_CURVE_WITH_KNOTS('',3,(#8082,#8083,#8084,#8085,#8086,#8087,
#8088,#8089,#8090,#8091,#8092,#8093,#8094,#8095,#8096,#8097,#8098,#8099,
#8100,#8101,#8102,#8103,#8104,#8105,#8106,#8107,#8108,#8109,#8110,#8111,
#8112,#8113,#8114,#8115,#8116,#8117,#8118,#8119,#8120,#8121,#8122,#8123,
#8124,#8125,#8126,#8127,#8128,#8129,#8130,#8131,#8132,#8133,#8134,#8135,
#8136,#8137,#8138,#8139,#8140,#8141,#8142,#8143,#8144,#8145,#8146,#8147,
#8148,#8149,#8150,#8151,#8152,#8153,#8154,#8155,#8156,#8157,#8158,#8159,
#8160,#8161,#8162,#8163,#8164,#8165,#8166,#8167,#8168,#8169,#8170,#8171,
#8172,#8173,#8174,#8175,#8176,#8177,#8178,#8179,#8180,#8181,#8182,#8183,
#8184,#8185,#8186,#8187,#8188,#8189,#8190,#8191,#8192,#8193,#8194,#8195,
#8196,#8197,#8198,#8199,#8200,#8201,#8202,#8203,#8204,#8205,#8206,#8207,
#8208,#8209,#8210,#8211,#8212,#8213,#8214,#8215,#8216,#8217,#8218,#8219,
#8220,#8221,#8222,#8223,#8224,#8225,#8226,#8227,#8228,#8229,#8230,#8231,
#8232,#8233,#8234,#8235,#8236,#8237,#8238,#8239,#8240,#8241,#8242,#8243,
#8244,#8245,#8246,#8247,#8248,#8249,#8250,#8251,#8252,#8253,#8254,#8255,
#8256,#8257,#8258,#8259,#8260,#8261,#8262,#8263,#8264,#8265,#8266,#8267,
#8268,#8269,#8270,#8271,#8272,#8273,#8274,#8275,#8276,#8277,#8278,#8279,
#8280,#8281,#8282,#8283,#8284,#8285,#8286,#8287,#8288,#8289,#8290,#8291,
#8292,#8293,#8294,#8295),.UNSPECIFIED.,.F.,.F.,(4,3,3,3,3,3,3,3,3,3,3,3,
3,3,3,3,3,3,3,3,3,3,3,3,3,3,3,3,3,3,3,3,3,3,3,3,3,3,3,3,3,3,3,3,3,3,3,3,
3,3,3,3,3,3,3,3,3,3,3,3,3,3,3,3,3,3,3,3,3,3,3,4),(0.00581528851415237,0.0198568721625981,
0.0211877409662844,0.0290621003554579,0.0370052281862515,0.0512291292287845,
0.0529041937053002,0.0644502614911372,0.0685278037786423,0.0841159711918372,
0.0919424126878769,0.0997790634725718,0.115448233246931,0.123085234974729,
0.131078038316822,0.146752253766709,0.162464053667518,0.178185986283123,
0.186042112011005,0.193890422727681,0.209550039573698,0.225138286678832,
0.240355181941911,0.240630028387911,0.248484045283646,0.256473909857358,
0.266662688666893,0.269672668683709,0.272111589151239,0.278265459195196,
0.284331412054608,0.288069318728516,0.298990155425507,0.303816384109195,
0.306319527110955,0.309583018903716,0.313229521738243,0.313648898796403,
0.319844455210027,0.325614289631532,0.328307642167298,0.332940771087925,
0.339713242837541,0.342966385538194,0.34605817259295,0.349007561947065,
0.350295757223643,0.357625128909093,0.364110633619828,0.372283872279993,
0.377813672911342,0.380677984752505,0.385953186130796,0.386942615650894,
0.395918491286659,0.401601359021794,0.408640030677264,0.411952448078052,
0.416260102392695,0.425748224011398,0.427444685160084,0.437067118782021,
0.443188392123352,0.445577589134499,0.458668272113456,0.4602363325054,0.467565704190851,
0.469398047112214,0.470772304303236,0.472833690089769,0.473864382983036,
0.474895075721047),.UNSPECIFIED.);
#45=B_SPLINE_SURFACE_WITH_KNOTS('',1,3,((#3726,#3727,#3728,#3729,#3730,
#3731,#3732,#3733,#3734,#3735,#3736,#3737,#3738,#3739,#3740,#3741,#3742,
#3743,#3744,#3745,#3746,#3747,#3748,#3749,#3750,#3751,#3752,#3753,#3754,
#3755,#3756,#3757,#3758,#3759,#3760,#3761,#3762,#3763,#3764,#3765,#3766,
#3767,#3768,#3769,#3770,#3771,#3772,#3773,#3774,#3775,#3776,#3777,#3778,
#3779,#3780,#3781,#3782,#3783,#3784,#3785,#3786,#3787,#3788,#3789,#3790,
#3791,#3792,#3793,#3794,#3795,#3796,#3797,#3798,#3799,#3800,#3801,#3802,
#3803,#3804,#3805,#3806,#3807,#3808,#3809,#3810,#3811,#3812,#3813,#3814,
#3815,#3816,#3817,#3818,#3819,#3820,#3821,#3822,#3823,#3824,#3825,#3826,
#3827,#3828,#3829,#3830,#3831,#3832,#3833,#3834,#3835,#3836,#3837,#3838,
#3839,#3840,#3841,#3842,#3843,#3844,#3845,#3846,#3847,#3848,#3849,#3850,
#3851,#3852,#3853,#3854,#3855,#3856,#3857,#3858,#3859,#3860,#3861,#3862,
#3863,#3864,#3865,#3866,#3867,#3868,#3869),(#3870,#3871,#3872,#3873,#3874,
#3875,#3876,#3877,#3878,#3879,#3880,#3881,#3882,#3883,#3884,#3885,#3886,
#3887,#3888,#3889,#3890,#3891,#3892,#3893,#3894,#3895,#3896,#3897,#3898,
#3899,#3900,#3901,#3902,#3903,#3904,#3905,#3906,#3907,#3908,#3909,#3910,
#3911,#3912,#3913,#3914,#3915,#3916,#3917,#3918,#3919,#3920,#3921,#3922,
#3923,#3924,#3925,#3926,#3927,#3928,#3929,#3930,#3931,#3932,#3933,#3934,
#3935,#3936,#3937,#3938,#3939,#3940,#3941,#3942,#3943,#3944,#3945,#3946,
#3947,#3948,#3949,#3950,#3951,#3952,#3953,#3954,#3955,#3956,#3957,#3958,
#3959,#3960,#3961,#3962,#3963,#3964,#3965,#3966,#3967,#3968,#3969,#3970,
#3971,#3972,#3973,#3974,#3975,#3976,#3977,#3978,#3979,#3980,#3981,#3982,
#3983,#3984,#3985,#3986,#3987,#3988,#3989,#3990,#3991,#3992,#3993,#3994,
#3995,#3996,#3997,#3998,#3999,#4000,#4001,#4002,#4003,#4004,#4005,#4006,
#4007,#4008,#4009,#4010,#4011,#4012,#4013)),.UNSPECIFIED.,.F.,.T.,.F.,(2,
2),(4,2,2,2,2,2,2,2,2,2,2,2,2,2,2,2,2,2,2,2,2,2,2,2,2,2,2,2,2,2,2,2,2,2,
2,2,2,2,2,2,2,2,2,2,2,2,2,2,2,2,2,2,2,2,2,2,2,2,2,2,2,2,2,2,2,2,2,2,2,2,
2,4),(0.,1.),(-4.79963010313954E-5,-1.80312514392642E-5,-3.04872664319862E-6,
1.1933798152867E-5,4.18988477449981E-5,7.18638973371293E-5,0.00010182894692926,
0.000116811471725326,0.000131793996521392,0.000161759046113523,0.000191724095705654,
0.000221689145297785,0.000251654194889916,0.000281619244482047,0.000296601769278113,
0.000311584294074179,0.00034154934366631,0.000371514393258441,0.000401479442850572,
0.000416461967646638,0.000431444492442703,0.000461409542034834,0.000491374591626965,
0.000521339641219097,0.000551304690811228,0.000581269740403359,0.00061123478999549,
0.000641199839587621,0.000671164889179752,0.000701129938771884,0.000731094988364015,
0.000761060037956146,0.000791025087548277,0.000820990137140408,0.000850955186732539,
0.000880920236324671,0.000910885285916802,0.000940850335508933,0.000970815385101064,
0.000985797909897129,0.0010007804346932,0.00103074548428533,0.00106071053387746,
0.00109067558346959,0.00110565810826565,0.00112064063306172,0.00115060568265385,
0.00118057073224598,0.00121053578183811,0.00124050083143024,0.00127046588102238,
0.00130043093061451,0.00133039598020664,0.00136036102979877,0.0013903260793909,
0.00142029112898303,0.00145025617857516,0.00148022122816729,0.00151018627775943,
0.00154015132735156,0.00157011637694369,0.00160008142653582,0.00163004647612795,
0.00166001152572008,0.00168997657531221,0.00171994162490434,0.00174990667449647,
0.00177987172408861,0.00180983677368074,0.0018248192984768,0.00183980182327287,
0.001869766872865),.UNSPECIFIED.);
#46=B_SPLINE_SURFACE_WITH_KNOTS('',1,3,((#7794,#7795,#7796,#7797,#7798,
#7799,#7800,#7801,#7802,#7803,#7804,#7805,#7806,#7807,#7808,#7809,#7810,
#7811,#7812,#7813,#7814,#7815,#7816,#7817,#7818,#7819,#7820,#7821,#7822,
#7823,#7824,#7825,#7826,#7827,#7828,#7829,#7830,#7831,#7832,#7833,#7834,
#7835,#7836,#7837,#7838,#7839,#7840,#7841,#7842,#7843,#7844,#7845,#7846,
#7847,#7848,#7849,#7850,#7851,#7852,#7853,#7854,#7855,#7856,#7857,#7858,
#7859,#7860,#7861,#7862,#7863,#7864,#7865,#7866,#7867,#7868,#7869,#7870,
#7871,#7872,#7873,#7874,#7875,#7876,#7877,#7878,#7879,#7880,#7881,#7882,
#7883,#7884,#7885,#7886,#7887,#7888,#7889,#7890,#7891,#7892,#7893,#7894,
#7895,#7896,#7897,#7898,#7899,#7900,#7901,#7902,#7903,#7904,#7905,#7906,
#7907,#7908,#7909,#7910,#7911,#7912,#7913,#7914,#7915,#7916,#7917,#7918,
#7919,#7920,#7921,#7922,#7923,#7924,#7925,#7926,#7927,#7928,#7929,#7930,
#7931,#7932,#7933,#7934,#7935,#7936,#7937),(#7938,#7939,#7940,#7941,#7942,
#7943,#7944,#7945,#7946,#7947,#7948,#7949,#7950,#7951,#7952,#7953,#7954,
#7955,#7956,#7957,#7958,#7959,#7960,#7961,#7962,#7963,#7964,#7965,#7966,
#7967,#7968,#7969,#7970,#7971,#7972,#7973,#7974,#7975,#7976,#7977,#7978,
#7979,#7980,#7981,#7982,#7983,#7984,#7985,#7986,#7987,#7988,#7989,#7990,
#7991,#7992,#7993,#7994,#7995,#7996,#7997,#7998,#7999,#8000,#8001,#8002,
#8003,#8004,#8005,#8006,#8007,#8008,#8009,#8010,#8011,#8012,#8013,#8014,
#8015,#8016,#8017,#8018,#8019,#8020,#8021,#8022,#8023,#8024,#8025,#8026,
#8027,#8028,#8029,#8030,#8031,#8032,#8033,#8034,#8035,#8036,#8037,#8038,
#8039,#8040,#8041,#8042,#8043,#8044,#8045,#8046,#8047,#8048,#8049,#8050,
#8051,#8052,#8053,#8054,#8055,#8056,#8057,#8058,#8059,#8060,#8061,#8062,
#8063,#8064,#8065,#8066,#8067,#8068,#8069,#8070,#8071,#8072,#8073,#8074,
#8075,#8076,#8077,#8078,#8079,#8080,#8081)),.UNSPECIFIED.,.F.,.T.,.F.,(2,
2),(4,2,2,2,2,2,2,2,2,2,2,2,2,2,2,2,2,2,2,2,2,2,2,2,2,2,2,2,2,2,2,2,2,2,
2,2,2,2,2,2,2,2,2,2,2,2,2,2,2,2,2,2,2,2,2,2,2,2,2,2,2,2,2,2,2,2,2,2,2,2,
2,4),(0.,1.),(-4.79963010313954E-5,-1.80312514392642E-5,-3.04872664319862E-6,
1.1933798152867E-5,4.18988477449981E-5,7.18638973371293E-5,0.00010182894692926,
0.000116811471725326,0.000131793996521392,0.000161759046113523,0.000191724095705654,
0.000221689145297785,0.000251654194889916,0.000281619244482047,0.000296601769278113,
0.000311584294074179,0.00034154934366631,0.000371514393258441,0.000401479442850572,
0.000416461967646638,0.000431444492442703,0.000461409542034834,0.000491374591626965,
0.000521339641219097,0.000551304690811228,0.000581269740403359,0.00061123478999549,
0.000641199839587621,0.000671164889179752,0.000701129938771884,0.000731094988364015,
0.000761060037956146,0.000791025087548277,0.000820990137140408,0.000850955186732539,
0.000880920236324671,0.000910885285916802,0.000940850335508933,0.000970815385101064,
0.000985797909897129,0.0010007804346932,0.00103074548428533,0.00106071053387746,
0.00109067558346959,0.00110565810826565,0.00112064063306172,0.00115060568265385,
0.00118057073224598,0.00121053578183811,0.00124050083143024,0.00127046588102238,
0.00130043093061451,0.00133039598020664,0.00136036102979877,0.0013903260793909,
0.00142029112898303,0.00145025617857516,0.00148022122816729,0.00151018627775943,
0.00154015132735156,0.00157011637694369,0.00160008142653582,0.00163004647612795,
0.00166001152572008,0.00168997657531221,0.00171994162490434,0.00174990667449647,
0.00177987172408861,0.00180983677368074,0.0018248192984768,0.00183980182327287,
0.001869766872865),.UNSPECIFIED.);
#47=SHAPE_REPRESENTATION_RELATIONSHIP('SRR','None',#9587,#53);
#48=SHAPE_REPRESENTATION_RELATIONSHIP('SRR','None',#9588,#54);
#49=SHAPE_REPRESENTATION_RELATIONSHIP('SRR','None',#9589,#55);
#50=SHAPE_REPRESENTATION_RELATIONSHIP('SRR','None',#9590,#56);
#51=SHAPE_REPRESENTATION_RELATIONSHIP('SRR','None',#9591,#57);
#52=SHAPE_REPRESENTATION_RELATIONSHIP('SRR','None',#9592,#58);
#53=ADVANCED_BREP_SHAPE_REPRESENTATION('',(#65),#9555);
#54=ADVANCED_BREP_SHAPE_REPRESENTATION('',(#66),#9556);
#55=ADVANCED_BREP_SHAPE_REPRESENTATION('',(#67),#9557);
#56=ADVANCED_BREP_SHAPE_REPRESENTATION('',(#68),#9558);
#57=ADVANCED_BREP_SHAPE_REPRESENTATION('',(#69),#9559);
#58=ADVANCED_BREP_SHAPE_REPRESENTATION('',(#70),#9560);
#59=STYLED_ITEM('',(#9626),#65);
#60=STYLED_ITEM('',(#9627),#66);
#61=STYLED_ITEM('',(#9628),#67);
#62=STYLED_ITEM('',(#9626),#68);
#63=STYLED_ITEM('',(#9629),#69);
#64=STYLED_ITEM('',(#9629),#70);
#65=MANIFOLD_SOLID_BREP('Body1',#2405);
#66=MANIFOLD_SOLID_BREP('Body1',#2406);
#67=MANIFOLD_SOLID_BREP('Body1',#2407);
#68=MANIFOLD_SOLID_BREP('Body1',#2408);
#69=MANIFOLD_SOLID_BREP('Body1',#2409);
#70=MANIFOLD_SOLID_BREP('Body1',#2410);
#71=FACE_BOUND('',#359,.T.);
#72=FACE_BOUND('',#361,.T.);
#73=FACE_BOUND('',#364,.T.);
#74=FACE_BOUND('',#365,.T.);
#75=FACE_BOUND('',#367,.T.);
#76=FACE_BOUND('',#368,.T.);
#77=FACE_BOUND('',#403,.T.);
#78=FACE_BOUND('',#405,.T.);
#79=FACE_BOUND('',#413,.T.);
#80=FACE_BOUND('',#419,.T.);
#81=FACE_BOUND('',#421,.T.);
#82=FACE_BOUND('',#423,.T.);
#83=FACE_BOUND('',#425,.T.);
#84=FACE_BOUND('',#444,.T.);
#85=FACE_BOUND('',#446,.T.);
#86=PLANE('',#2504);
#87=PLANE('',#2505);
#88=PLANE('',#2509);
#89=PLANE('',#2510);
#90=PLANE('',#2514);
#91=PLANE('',#2515);
#92=PLANE('',#2516);
#93=PLANE('',#2526);
#94=PLANE('',#2527);
#95=PLANE('',#2528);
#96=PLANE('',#2532);
#97=PLANE('',#2534);
#98=PLANE('',#2537);
#99=PLANE('',#2538);
#100=PLANE('',#2558);
#101=PLANE('',#2559);
#102=PLANE('',#2560);
#103=PLANE('',#2561);
#104=PLANE('',#2562);
#105=PLANE('',#2563);
#106=PLANE('',#2564);
#107=PLANE('',#2568);
#108=PLANE('',#2569);
#109=PLANE('',#2570);
#110=PLANE('',#2571);
#111=PLANE('',#2572);
#112=PLANE('',#2573);
#113=PLANE('',#2574);
#114=PLANE('',#2575);
#115=PLANE('',#2576);
#116=PLANE('',#2578);
#117=PLANE('',#2579);
#118=PLANE('',#2582);
#119=PLANE('',#2583);
#120=PLANE('',#2584);
#121=PLANE('',#2585);
#122=PLANE('',#2586);
#123=PLANE('',#2587);
#124=PLANE('',#2588);
#125=PLANE('',#2589);
#126=PLANE('',#2604);
#127=PLANE('',#2605);
#128=PLANE('',#2606);
#129=PLANE('',#2607);
#130=PLANE('',#2608);
#131=PLANE('',#2609);
#132=PLANE('',#2610);
#133=PLANE('',#2611);
#134=PLANE('',#2612);
#135=PLANE('',#2617);
#136=PLANE('',#2618);
#137=PLANE('',#2619);
#138=PLANE('',#2620);
#139=PLANE('',#2621);
#140=PLANE('',#2622);
#141=PLANE('',#2623);
#142=PLANE('',#2624);
#143=PLANE('',#2625);
#144=PLANE('',#2626);
#145=PLANE('',#2627);
#146=PLANE('',#2628);
#147=PLANE('',#2629);
#148=PLANE('',#2630);
#149=PLANE('',#2633);
#150=PLANE('',#2638);
#151=PLANE('',#2639);
#152=PLANE('',#2640);
#153=PLANE('',#2641);
#154=PLANE('',#2642);
#155=PLANE('',#2643);
#156=PLANE('',#2644);
#157=PLANE('',#2645);
#158=PLANE('',#2646);
#159=PLANE('',#2647);
#160=PLANE('',#2648);
#161=PLANE('',#2649);
#162=PLANE('',#2650);
#163=PLANE('',#2651);
#164=PLANE('',#2652);
#165=PLANE('',#2653);
#166=PLANE('',#2654);
#167=PLANE('',#2655);
#168=PLANE('',#2656);
#169=PLANE('',#2657);
#170=PLANE('',#2658);
#171=PLANE('',#2659);
#172=PLANE('',#2660);
#173=PLANE('',#2661);
#174=PLANE('',#2662);
#175=PLANE('',#2663);
#176=PLANE('',#2664);
#177=PLANE('',#2665);
#178=PLANE('',#2666);
#179=PLANE('',#2667);
#180=PLANE('',#2668);
#181=PLANE('',#2669);
#182=PLANE('',#2670);
#183=PLANE('',#2671);
#184=PLANE('',#2672);
#185=PLANE('',#2673);
#186=PLANE('',#2674);
#187=PLANE('',#2675);
#188=PLANE('',#2676);
#189=PLANE('',#2677);
#190=PLANE('',#2682);
#191=PLANE('',#2683);
#192=PLANE('',#2688);
#193=PLANE('',#2689);
#194=FACE_OUTER_BOUND('',#337,.T.);
#195=FACE_OUTER_BOUND('',#338,.T.);
#196=FACE_OUTER_BOUND('',#339,.T.);
#197=FACE_OUTER_BOUND('',#340,.T.);
#198=FACE_OUTER_BOUND('',#341,.T.);
#199=FACE_OUTER_BOUND('',#342,.T.);
#200=FACE_OUTER_BOUND('',#343,.T.);
#201=FACE_OUTER_BOUND('',#344,.T.);
#202=FACE_OUTER_BOUND('',#345,.T.);
#203=FACE_OUTER_BOUND('',#346,.T.);
#204=FACE_OUTER_BOUND('',#347,.T.);
#205=FACE_OUTER_BOUND('',#348,.T.);
#206=FACE_OUTER_BOUND('',#349,.T.);
#207=FACE_OUTER_BOUND('',#350,.T.);
#208=FACE_OUTER_BOUND('',#351,.T.);
#209=FACE_OUTER_BOUND('',#352,.T.);
#210=FACE_OUTER_BOUND('',#353,.T.);
#211=FACE_OUTER_BOUND('',#354,.T.);
#212=FACE_OUTER_BOUND('',#355,.T.);
#213=FACE_OUTER_BOUND('',#356,.T.);
#214=FACE_OUTER_BOUND('',#357,.T.);
#215=FACE_OUTER_BOUND('',#358,.T.);
#216=FACE_OUTER_BOUND('',#360,.T.);
#217=FACE_OUTER_BOUND('',#362,.T.);
#218=FACE_OUTER_BOUND('',#363,.T.);
#219=FACE_OUTER_BOUND('',#366,.T.);
#220=FACE_OUTER_BOUND('',#369,.T.);
#221=FACE_OUTER_BOUND('',#370,.T.);
#222=FACE_OUTER_BOUND('',#371,.T.);
#223=FACE_OUTER_BOUND('',#372,.T.);
#224=FACE_OUTER_BOUND('',#373,.T.);
#225=FACE_OUTER_BOUND('',#374,.T.);
#226=FACE_OUTER_BOUND('',#375,.T.);
#227=FACE_OUTER_BOUND('',#376,.T.);
#228=FACE_OUTER_BOUND('',#377,.T.);
#229=FACE_OUTER_BOUND('',#378,.T.);
#230=FACE_OUTER_BOUND('',#379,.T.);
#231=FACE_OUTER_BOUND('',#380,.T.);
#232=FACE_OUTER_BOUND('',#381,.T.);
#233=FACE_OUTER_BOUND('',#382,.T.);
#234=FACE_OUTER_BOUND('',#383,.T.);
#235=FACE_OUTER_BOUND('',#384,.T.);
#236=FACE_OUTER_BOUND('',#385,.T.);
#237=FACE_OUTER_BOUND('',#386,.T.);
#238=FACE_OUTER_BOUND('',#387,.T.);
#239=FACE_OUTER_BOUND('',#388,.T.);
#240=FACE_OUTER_BOUND('',#389,.T.);
#241=FACE_OUTER_BOUND('',#390,.T.);
#242=FACE_OUTER_BOUND('',#391,.T.);
#243=FACE_OUTER_BOUND('',#392,.T.);
#244=FACE_OUTER_BOUND('',#393,.T.);
#245=FACE_OUTER_BOUND('',#394,.T.);
#246=FACE_OUTER_BOUND('',#395,.T.);
#247=FACE_OUTER_BOUND('',#396,.T.);
#248=FACE_OUTER_BOUND('',#397,.T.);
#249=FACE_OUTER_BOUND('',#398,.T.);
#250=FACE_OUTER_BOUND('',#399,.T.);
#251=FACE_OUTER_BOUND('',#400,.T.);
#252=FACE_OUTER_BOUND('',#401,.T.);
#253=FACE_OUTER_BOUND('',#402,.T.);
#254=FACE_OUTER_BOUND('',#404,.T.);
#255=FACE_OUTER_BOUND('',#406,.T.);
#256=FACE_OUTER_BOUND('',#407,.T.);
#257=FACE_OUTER_BOUND('',#408,.T.);
#258=FACE_OUTER_BOUND('',#409,.T.);
#259=FACE_OUTER_BOUND('',#410,.T.);
#260=FACE_OUTER_BOUND('',#411,.T.);
#261=FACE_OUTER_BOUND('',#412,.T.);
#262=FACE_OUTER_BOUND('',#414,.T.);
#263=FACE_OUTER_BOUND('',#415,.T.);
#264=FACE_OUTER_BOUND('',#416,.T.);
#265=FACE_OUTER_BOUND('',#417,.T.);
#266=FACE_OUTER_BOUND('',#418,.T.);
#267=FACE_OUTER_BOUND('',#420,.T.);
#268=FACE_OUTER_BOUND('',#422,.T.);
#269=FACE_OUTER_BOUND('',#424,.T.);
#270=FACE_OUTER_BOUND('',#426,.T.);
#271=FACE_OUTER_BOUND('',#427,.T.);
#272=FACE_OUTER_BOUND('',#428,.T.);
#273=FACE_OUTER_BOUND('',#429,.T.);
#274=FACE_OUTER_BOUND('',#430,.T.);
#275=FACE_OUTER_BOUND('',#431,.T.);
#276=FACE_OUTER_BOUND('',#432,.T.);
#277=FACE_OUTER_BOUND('',#433,.T.);
#278=FACE_OUTER_BOUND('',#434,.T.);
#279=FACE_OUTER_BOUND('',#435,.T.);
#280=FACE_OUTER_BOUND('',#436,.T.);
#281=FACE_OUTER_BOUND('',#437,.T.);
#282=FACE_OUTER_BOUND('',#438,.T.);
#283=FACE_OUTER_BOUND('',#439,.T.);
#284=FACE_OUTER_BOUND('',#440,.T.);
#285=FACE_OUTER_BOUND('',#441,.T.);
#286=FACE_OUTER_BOUND('',#442,.T.);
#287=FACE_OUTER_BOUND('',#443,.T.);
#288=FACE_OUTER_BOUND('',#445,.T.);
#289=FACE_OUTER_BOUND('',#447,.T.);
#290=FACE_OUTER_BOUND('',#448,.T.);
#291=FACE_OUTER_BOUND('',#449,.T.);
#292=FACE_OUTER_BOUND('',#450,.T.);
#293=FACE_OUTER_BOUND('',#451,.T.);
#294=FACE_OUTER_BOUND('',#452,.T.);
#295=FACE_OUTER_BOUND('',#453,.T.);
#296=FACE_OUTER_BOUND('',#454,.T.);
#297=FACE_OUTER_BOUND('',#455,.T.);
#298=FACE_OUTER_BOUND('',#456,.T.);
#299=FACE_OUTER_BOUND('',#457,.T.);
#300=FACE_OUTER_BOUND('',#458,.T.);
#301=FACE_OUTER_BOUND('',#459,.T.);
#302=FACE_OUTER_BOUND('',#460,.T.);
#303=FACE_OUTER_BOUND('',#461,.T.);
#304=FACE_OUTER_BOUND('',#462,.T.);
#305=FACE_OUTER_BOUND('',#463,.T.);
#306=FACE_OUTER_BOUND('',#464,.T.);
#307=FACE_OUTER_BOUND('',#465,.T.);
#308=FACE_OUTER_BOUND('',#466,.T.);
#309=FACE_OUTER_BOUND('',#467,.T.);
#310=FACE_OUTER_BOUND('',#468,.T.);
#311=FACE_OUTER_BOUND('',#469,.T.);
#312=FACE_OUTER_BOUND('',#470,.T.);
#313=FACE_OUTER_BOUND('',#471,.T.);
#314=FACE_OUTER_BOUND('',#472,.T.);
#315=FACE_OUTER_BOUND('',#473,.T.);
#316=FACE_OUTER_BOUND('',#474,.T.);
#317=FACE_OUTER_BOUND('',#475,.T.);
#318=FACE_OUTER_BOUND('',#476,.T.);
#319=FACE_OUTER_BOUND('',#477,.T.);
#320=FACE_OUTER_BOUND('',#478,.T.);
#321=FACE_OUTER_BOUND('',#479,.T.);
#322=FACE_OUTER_BOUND('',#480,.T.);
#323=FACE_OUTER_BOUND('',#481,.T.);
#324=FACE_OUTER_BOUND('',#482,.T.);
#325=FACE_OUTER_BOUND('',#483,.T.);
#326=FACE_OUTER_BOUND('',#484,.T.);
#327=FACE_OUTER_BOUND('',#485,.T.);
#328=FACE_OUTER_BOUND('',#486,.T.);
#329=FACE_OUTER_BOUND('',#487,.T.);
#330=FACE_OUTER_BOUND('',#488,.T.);
#331=FACE_OUTER_BOUND('',#489,.T.);
#332=FACE_OUTER_BOUND('',#490,.T.);
#333=FACE_OUTER_BOUND('',#491,.T.);
#334=FACE_OUTER_BOUND('',#492,.T.);
#335=FACE_OUTER_BOUND('',#493,.T.);
#336=FACE_OUTER_BOUND('',#494,.T.);
#337=EDGE_LOOP('',(#1583,#1584,#1585,#1586));
#338=EDGE_LOOP('',(#1587,#1588,#1589,#1590));
#339=EDGE_LOOP('',(#1591,#1592,#1593,#1594));
#340=EDGE_LOOP('',(#1595,#1596,#1597,#1598));
#341=EDGE_LOOP('',(#1599,#1600,#1601,#1602));
#342=EDGE_LOOP('',(#1603,#1604,#1605,#1606));
#343=EDGE_LOOP('',(#1607,#1608,#1609,#1610));
#344=EDGE_LOOP('',(#1611,#1612,#1613,#1614));
#345=EDGE_LOOP('',(#1615,#1616,#1617,#1618));
#346=EDGE_LOOP('',(#1619,#1620,#1621,#1622));
#347=EDGE_LOOP('',(#1623,#1624,#1625,#1626));
#348=EDGE_LOOP('',(#1627,#1628,#1629,#1630,#1631,#1632,#1633,#1634));
#349=EDGE_LOOP('',(#1635,#1636,#1637,#1638,#1639,#1640,#1641,#1642));
#350=EDGE_LOOP('',(#1643,#1644,#1645,#1646));
#351=EDGE_LOOP('',(#1647,#1648,#1649,#1650));
#352=EDGE_LOOP('',(#1651,#1652,#1653,#1654));
#353=EDGE_LOOP('',(#1655,#1656,#1657,#1658));
#354=EDGE_LOOP('',(#1659,#1660,#1661,#1662));
#355=EDGE_LOOP('',(#1663,#1664,#1665,#1666));
#356=EDGE_LOOP('',(#1667,#1668,#1669,#1670));
#357=EDGE_LOOP('',(#1671,#1672,#1673,#1674));
#358=EDGE_LOOP('',(#1675,#1676,#1677,#1678,#1679,#1680,#1681,#1682,#1683,
#1684));
#359=EDGE_LOOP('',(#1685));
#360=EDGE_LOOP('',(#1686,#1687,#1688,#1689,#1690,#1691,#1692,#1693,#1694,
#1695));
#361=EDGE_LOOP('',(#1696));
#362=EDGE_LOOP('',(#1697,#1698,#1699,#1700));
#363=EDGE_LOOP('',(#1701,#1702,#1703,#1704,#1705,#1706,#1707,#1708,#1709,
#1710,#1711));
#364=EDGE_LOOP('',(#1712));
#365=EDGE_LOOP('',(#1713));
#366=EDGE_LOOP('',(#1714,#1715,#1716,#1717,#1718,#1719,#1720,#1721,#1722,
#1723,#1724));
#367=EDGE_LOOP('',(#1725));
#368=EDGE_LOOP('',(#1726));
#369=EDGE_LOOP('',(#1727,#1728,#1729,#1730));
#370=EDGE_LOOP('',(#1731));
#371=EDGE_LOOP('',(#1732));
#372=EDGE_LOOP('',(#1733,#1734,#1735,#1736));
#373=EDGE_LOOP('',(#1737,#1738,#1739,#1740));
#374=EDGE_LOOP('',(#1741,#1742,#1743,#1744));
#375=EDGE_LOOP('',(#1745,#1746,#1747,#1748));
#376=EDGE_LOOP('',(#1749,#1750,#1751,#1752));
#377=EDGE_LOOP('',(#1753,#1754,#1755,#1756));
#378=EDGE_LOOP('',(#1757,#1758,#1759,#1760));
#379=EDGE_LOOP('',(#1761,#1762,#1763,#1764));
#380=EDGE_LOOP('',(#1765,#1766,#1767,#1768));
#381=EDGE_LOOP('',(#1769,#1770,#1771,#1772));
#382=EDGE_LOOP('',(#1773,#1774,#1775,#1776));
#383=EDGE_LOOP('',(#1777,#1778,#1779,#1780));
#384=EDGE_LOOP('',(#1781,#1782,#1783,#1784,#1785,#1786,#1787,#1788));
#385=EDGE_LOOP('',(#1789,#1790,#1791,#1792));
#386=EDGE_LOOP('',(#1793,#1794,#1795,#1796,#1797,#1798,#1799,#1800));
#387=EDGE_LOOP('',(#1801,#1802,#1803,#1804));
#388=EDGE_LOOP('',(#1805,#1806,#1807,#1808));
#389=EDGE_LOOP('',(#1809,#1810,#1811,#1812));
#390=EDGE_LOOP('',(#1813,#1814,#1815,#1816));
#391=EDGE_LOOP('',(#1817,#1818,#1819,#1820));
#392=EDGE_LOOP('',(#1821,#1822,#1823,#1824));
#393=EDGE_LOOP('',(#1825,#1826,#1827,#1828));
#394=EDGE_LOOP('',(#1829,#1830,#1831,#1832,#1833,#1834,#1835,#1836,#1837,
#1838,#1839,#1840,#1841));
#395=EDGE_LOOP('',(#1842,#1843,#1844,#1845,#1846,#1847,#1848,#1849,#1850,
#1851,#1852,#1853,#1854));
#396=EDGE_LOOP('',(#1855,#1856,#1857,#1858,#1859,#1860,#1861,#1862));
#397=EDGE_LOOP('',(#1863,#1864,#1865,#1866));
#398=EDGE_LOOP('',(#1867,#1868,#1869,#1870));
#399=EDGE_LOOP('',(#1871,#1872,#1873,#1874));
#400=EDGE_LOOP('',(#1875,#1876,#1877,#1878));
#401=EDGE_LOOP('',(#1879,#1880,#1881,#1882));
#402=EDGE_LOOP('',(#1883,#1884,#1885,#1886,#1887,#1888,#1889,#1890,#1891,
#1892,#1893,#1894,#1895,#1896,#1897));
#403=EDGE_LOOP('',(#1898));
#404=EDGE_LOOP('',(#1899,#1900,#1901,#1902,#1903,#1904,#1905,#1906,#1907,
#1908,#1909,#1910,#1911,#1912,#1913));
#405=EDGE_LOOP('',(#1914));
#406=EDGE_LOOP('',(#1915));
#407=EDGE_LOOP('',(#1916));
#408=EDGE_LOOP('',(#1917,#1918,#1919,#1920,#1921));
#409=EDGE_LOOP('',(#1922,#1923,#1924,#1925,#1926));
#410=EDGE_LOOP('',(#1927,#1928,#1929,#1930));
#411=EDGE_LOOP('',(#1931,#1932,#1933,#1934));
#412=EDGE_LOOP('',(#1935,#1936,#1937,#1938));
#413=EDGE_LOOP('',(#1939,#1940,#1941,#1942));
#414=EDGE_LOOP('',(#1943,#1944,#1945,#1946));
#415=EDGE_LOOP('',(#1947,#1948,#1949,#1950));
#416=EDGE_LOOP('',(#1951,#1952,#1953,#1954));
#417=EDGE_LOOP('',(#1955,#1956,#1957,#1958));
#418=EDGE_LOOP('',(#1959));
#419=EDGE_LOOP('',(#1960));
#420=EDGE_LOOP('',(#1961));
#421=EDGE_LOOP('',(#1962));
#422=EDGE_LOOP('',(#1963));
#423=EDGE_LOOP('',(#1964,#1965,#1966,#1967));
#424=EDGE_LOOP('',(#1968));
#425=EDGE_LOOP('',(#1969,#1970));
#426=EDGE_LOOP('',(#1971,#1972));
#427=EDGE_LOOP('',(#1973,#1974,#1975,#1976,#1977));
#428=EDGE_LOOP('',(#1978,#1979,#1980,#1981,#1982));
#429=EDGE_LOOP('',(#1983,#1984,#1985,#1986));
#430=EDGE_LOOP('',(#1987,#1988,#1989,#1990));
#431=EDGE_LOOP('',(#1991,#1992,#1993,#1994));
#432=EDGE_LOOP('',(#1995,#1996,#1997,#1998));
#433=EDGE_LOOP('',(#1999,#2000,#2001,#2002));
#434=EDGE_LOOP('',(#2003,#2004,#2005,#2006));
#435=EDGE_LOOP('',(#2007,#2008,#2009,#2010));
#436=EDGE_LOOP('',(#2011,#2012,#2013,#2014));
#437=EDGE_LOOP('',(#2015,#2016,#2017,#2018));
#438=EDGE_LOOP('',(#2019,#2020,#2021,#2022));
#439=EDGE_LOOP('',(#2023,#2024,#2025,#2026));
#440=EDGE_LOOP('',(#2027,#2028,#2029,#2030));
#441=EDGE_LOOP('',(#2031,#2032,#2033,#2034));
#442=EDGE_LOOP('',(#2035,#2036,#2037,#2038));
#443=EDGE_LOOP('',(#2039,#2040,#2041,#2042,#2043,#2044,#2045,#2046,#2047,
#2048,#2049,#2050,#2051,#2052,#2053,#2054,#2055,#2056,#2057,#2058,#2059,
#2060,#2061,#2062,#2063));
#444=EDGE_LOOP('',(#2064));
#445=EDGE_LOOP('',(#2065,#2066,#2067,#2068,#2069,#2070,#2071,#2072,#2073,
#2074,#2075,#2076,#2077,#2078,#2079,#2080,#2081,#2082,#2083,#2084,#2085,
#2086,#2087,#2088,#2089));
#446=EDGE_LOOP('',(#2090));
#447=EDGE_LOOP('',(#2091,#2092,#2093,#2094));
#448=EDGE_LOOP('',(#2095,#2096,#2097,#2098));
#449=EDGE_LOOP('',(#2099,#2100,#2101));
#450=EDGE_LOOP('',(#2102,#2103,#2104));
#451=EDGE_LOOP('',(#2105,#2106,#2107));
#452=EDGE_LOOP('',(#2108,#2109,#2110));
#453=EDGE_LOOP('',(#2111,#2112,#2113));
#454=EDGE_LOOP('',(#2114,#2115,#2116));
#455=EDGE_LOOP('',(#2117,#2118,#2119));
#456=EDGE_LOOP('',(#2120,#2121,#2122));
#457=EDGE_LOOP('',(#2123,#2124,#2125));
#458=EDGE_LOOP('',(#2126,#2127,#2128));
#459=EDGE_LOOP('',(#2129,#2130,#2131));
#460=EDGE_LOOP('',(#2132,#2133,#2134));
#461=EDGE_LOOP('',(#2135,#2136,#2137));
#462=EDGE_LOOP('',(#2138,#2139,#2140));
#463=EDGE_LOOP('',(#2141,#2142,#2143));
#464=EDGE_LOOP('',(#2144,#2145,#2146));
#465=EDGE_LOOP('',(#2147,#2148,#2149));
#466=EDGE_LOOP('',(#2150,#2151,#2152));
#467=EDGE_LOOP('',(#2153,#2154,#2155));
#468=EDGE_LOOP('',(#2156,#2157,#2158));
#469=EDGE_LOOP('',(#2159,#2160,#2161));
#470=EDGE_LOOP('',(#2162,#2163,#2164));
#471=EDGE_LOOP('',(#2165,#2166,#2167));
#472=EDGE_LOOP('',(#2168,#2169,#2170));
#473=EDGE_LOOP('',(#2171,#2172,#2173));
#474=EDGE_LOOP('',(#2174,#2175,#2176));
#475=EDGE_LOOP('',(#2177,#2178,#2179));
#476=EDGE_LOOP('',(#2180,#2181,#2182));
#477=EDGE_LOOP('',(#2183,#2184,#2185));
#478=EDGE_LOOP('',(#2186,#2187,#2188));
#479=EDGE_LOOP('',(#2189,#2190,#2191));
#480=EDGE_LOOP('',(#2192,#2193,#2194));
#481=EDGE_LOOP('',(#2195,#2196,#2197));
#482=EDGE_LOOP('',(#2198,#2199,#2200));
#483=EDGE_LOOP('',(#2201,#2202,#2203));
#484=EDGE_LOOP('',(#2204,#2205,#2206));
#485=EDGE_LOOP('',(#2207,#2208,#2209));
#486=EDGE_LOOP('',(#2210,#2211,#2212));
#487=EDGE_LOOP('',(#2213,#2214,#2215));
#488=EDGE_LOOP('',(#2216,#2217,#2218));
#489=EDGE_LOOP('',(#2219,#2220,#2221,#2222));
#490=EDGE_LOOP('',(#2223));
#491=EDGE_LOOP('',(#2224));
#492=EDGE_LOOP('',(#2225,#2226,#2227,#2228));
#493=EDGE_LOOP('',(#2229));
#494=EDGE_LOOP('',(#2230));
#495=LINE('',#3388,#745);
#496=LINE('',#3394,#746);
#497=LINE('',#3400,#747);
#498=LINE('',#3406,#748);
#499=LINE('',#3413,#749);
#500=LINE('',#3416,#750);
#501=LINE('',#3422,#751);
#502=LINE('',#3425,#752);
#503=LINE('',#3431,#753);
#504=LINE('',#3434,#754);
#505=LINE('',#3440,#755);
#506=LINE('',#3443,#756);
#507=LINE('',#3447,#757);
#508=LINE('',#3449,#758);
#509=LINE('',#3451,#759);
#510=LINE('',#3452,#760);
#511=LINE('',#3455,#761);
#512=LINE('',#3457,#762);
#513=LINE('',#3458,#763);
#514=LINE('',#3464,#764);
#515=LINE('',#3468,#765);
#516=LINE('',#3469,#766);
#517=LINE('',#3471,#767);
#518=LINE('',#3473,#768);
#519=LINE('',#3475,#769);
#520=LINE('',#3477,#770);
#521=LINE('',#3478,#771);
#522=LINE('',#3480,#772);
#523=LINE('',#3481,#773);
#524=LINE('',#3482,#774);
#525=LINE('',#3483,#775);
#526=LINE('',#3489,#776);
#527=LINE('',#3491,#777);
#528=LINE('',#3492,#778);
#529=LINE('',#3496,#779);
#530=LINE('',#3498,#780);
#531=LINE('',#3500,#781);
#532=LINE('',#3501,#782);
#533=LINE('',#3504,#783);
#534=LINE('',#3506,#784);
#535=LINE('',#3507,#785);
#536=LINE('',#3518,#786);
#537=LINE('',#3521,#787);
#538=LINE('',#3522,#788);
#539=LINE('',#3529,#789);
#540=LINE('',#3543,#790);
#541=LINE('',#3549,#791);
#542=LINE('',#3556,#792);
#543=LINE('',#3559,#793);
#544=LINE('',#3565,#794);
#545=LINE('',#3568,#795);
#546=LINE('',#3574,#796);
#547=LINE('',#3577,#797);
#548=LINE('',#3583,#798);
#549=LINE('',#3586,#799);
#550=LINE('',#3589,#800);
#551=LINE('',#3591,#801);
#552=LINE('',#3592,#802);
#553=LINE('',#3595,#803);
#554=LINE('',#3597,#804);
#555=LINE('',#3598,#805);
#556=LINE('',#3601,#806);
#557=LINE('',#3603,#807);
#558=LINE('',#3604,#808);
#559=LINE('',#3607,#809);
#560=LINE('',#3609,#810);
#561=LINE('',#3610,#811);
#562=LINE('',#3613,#812);
#563=LINE('',#3615,#813);
#564=LINE('',#3616,#814);
#565=LINE('',#3619,#815);
#566=LINE('',#3621,#816);
#567=LINE('',#3622,#817);
#568=LINE('',#3625,#818);
#569=LINE('',#3627,#819);
#570=LINE('',#3629,#820);
#571=LINE('',#3631,#821);
#572=LINE('',#3633,#822);
#573=LINE('',#3635,#823);
#574=LINE('',#3636,#824);
#575=LINE('',#3641,#825);
#576=LINE('',#3644,#826);
#577=LINE('',#3645,#827);
#578=LINE('',#3646,#828);
#579=LINE('',#3647,#829);
#580=LINE('',#3650,#830);
#581=LINE('',#3652,#831);
#582=LINE('',#3653,#832);
#583=LINE('',#3656,#833);
#584=LINE('',#3658,#834);
#585=LINE('',#3659,#835);
#586=LINE('',#3662,#836);
#587=LINE('',#3664,#837);
#588=LINE('',#3665,#838);
#589=LINE('',#3668,#839);
#590=LINE('',#3670,#840);
#591=LINE('',#3671,#841);
#592=LINE('',#3674,#842);
#593=LINE('',#3676,#843);
#594=LINE('',#3677,#844);
#595=LINE('',#3679,#845);
#596=LINE('',#3680,#846);
#597=LINE('',#3683,#847);
#598=LINE('',#3685,#848);
#599=LINE('',#3686,#849);
#600=LINE('',#3690,#850);
#601=LINE('',#3692,#851);
#602=LINE('',#3696,#852);
#603=LINE('',#3697,#853);
#604=LINE('',#3699,#854);
#605=LINE('',#3700,#855);
#606=LINE('',#3705,#856);
#607=LINE('',#3707,#857);
#608=LINE('',#3708,#858);
#609=LINE('',#3711,#859);
#610=LINE('',#3713,#860);
#611=LINE('',#3714,#861);
#612=LINE('',#3716,#862);
#613=LINE('',#3717,#863);
#614=LINE('',#3719,#864);
#615=LINE('',#3720,#865);
#616=LINE('',#4243,#866);
#617=LINE('',#4266,#867);
#618=LINE('',#7707,#868);
#619=LINE('',#7713,#869);
#620=LINE('',#7719,#870);
#621=LINE('',#7725,#871);
#622=LINE('',#7728,#872);
#623=LINE('',#7732,#873);
#624=LINE('',#7733,#874);
#625=LINE('',#7734,#875);
#626=LINE('',#7737,#876);
#627=LINE('',#7739,#877);
#628=LINE('',#7740,#878);
#629=LINE('',#7742,#879);
#630=LINE('',#7744,#880);
#631=LINE('',#9288,#881);
#632=LINE('',#9293,#882);
#633=LINE('',#9295,#883);
#634=LINE('',#9297,#884);
#635=LINE('',#9298,#885);
#636=LINE('',#9302,#886);
#637=LINE('',#9304,#887);
#638=LINE('',#9306,#888);
#639=LINE('',#9307,#889);
#640=LINE('',#9311,#890);
#641=LINE('',#9313,#891);
#642=LINE('',#9315,#892);
#643=LINE('',#9316,#893);
#644=LINE('',#9320,#894);
#645=LINE('',#9322,#895);
#646=LINE('',#9324,#896);
#647=LINE('',#9325,#897);
#648=LINE('',#9329,#898);
#649=LINE('',#9331,#899);
#650=LINE('',#9333,#900);
#651=LINE('',#9334,#901);
#652=LINE('',#9338,#902);
#653=LINE('',#9340,#903);
#654=LINE('',#9342,#904);
#655=LINE('',#9343,#905);
#656=LINE('',#9347,#906);
#657=LINE('',#9349,#907);
#658=LINE('',#9351,#908);
#659=LINE('',#9352,#909);
#660=LINE('',#9356,#910);
#661=LINE('',#9358,#911);
#662=LINE('',#9360,#912);
#663=LINE('',#9361,#913);
#664=LINE('',#9365,#914);
#665=LINE('',#9367,#915);
#666=LINE('',#9369,#916);
#667=LINE('',#9370,#917);
#668=LINE('',#9374,#918);
#669=LINE('',#9376,#919);
#670=LINE('',#9378,#920);
#671=LINE('',#9379,#921);
#672=LINE('',#9383,#922);
#673=LINE('',#9385,#923);
#674=LINE('',#9387,#924);
#675=LINE('',#9388,#925);
#676=LINE('',#9391,#926);
#677=LINE('',#9393,#927);
#678=LINE('',#9394,#928);
#679=LINE('',#9397,#929);
#680=LINE('',#9399,#930);
#681=LINE('',#9400,#931);
#682=LINE('',#9402,#932);
#683=LINE('',#9403,#933);
#684=LINE('',#9404,#934);
#685=LINE('',#9405,#935);
#686=LINE('',#9406,#936);
#687=LINE('',#9407,#937);
#688=LINE('',#9408,#938);
#689=LINE('',#9409,#939);
#690=LINE('',#9410,#940);
#691=LINE('',#9411,#941);
#692=LINE('',#9416,#942);
#693=LINE('',#9417,#943);
#694=LINE('',#9418,#944);
#695=LINE('',#9419,#945);
#696=LINE('',#9420,#946);
#697=LINE('',#9421,#947);
#698=LINE('',#9422,#948);
#699=LINE('',#9423,#949);
#700=LINE('',#9424,#950);
#701=LINE('',#9425,#951);
#702=LINE('',#9430,#952);
#703=LINE('',#9434,#953);
#704=LINE('',#9435,#954);
#705=LINE('',#9437,#955);
#706=LINE('',#9439,#956);
#707=LINE('',#9443,#957);
#708=LINE('',#9444,#958);
#709=LINE('',#9446,#959);
#710=LINE('',#9448,#960);
#711=LINE('',#9452,#961);
#712=LINE('',#9453,#962);
#713=LINE('',#9455,#963);
#714=LINE('',#9457,#964);
#715=LINE('',#9461,#965);
#716=LINE('',#9462,#966);
#717=LINE('',#9464,#967);
#718=LINE('',#9466,#968);
#719=LINE('',#9470,#969);
#720=LINE('',#9471,#970);
#721=LINE('',#9473,#971);
#722=LINE('',#9475,#972);
#723=LINE('',#9479,#973);
#724=LINE('',#9480,#974);
#725=LINE('',#9482,#975);
#726=LINE('',#9484,#976);
#727=LINE('',#9488,#977);
#728=LINE('',#9489,#978);
#729=LINE('',#9491,#979);
#730=LINE('',#9493,#980);
#731=LINE('',#9497,#981);
#732=LINE('',#9498,#982);
#733=LINE('',#9500,#983);
#734=LINE('',#9502,#984);
#735=LINE('',#9506,#985);
#736=LINE('',#9507,#986);
#737=LINE('',#9509,#987);
#738=LINE('',#9511,#988);
#739=LINE('',#9515,#989);
#740=LINE('',#9516,#990);
#741=LINE('',#9518,#991);
#742=LINE('',#9520,#992);
#743=LINE('',#9527,#993);
#744=LINE('',#9536,#994);
#745=VECTOR('',#2704,1.25);
#746=VECTOR('',#2711,1.25);
#747=VECTOR('',#2718,1.5);
#748=VECTOR('',#2725,1.5);
#749=VECTOR('',#2732,1000.);
#750=VECTOR('',#2735,1000.);
#751=VECTOR('',#2740,1000.);
#752=VECTOR('',#2743,1000.);
#753=VECTOR('',#2748,1000.);
#754=VECTOR('',#2751,1000.);
#755=VECTOR('',#2756,1000.);
#756=VECTOR('',#2759,1000.);
#757=VECTOR('',#2762,1000.);
#758=VECTOR('',#2763,1000.);
#759=VECTOR('',#2764,1000.);
#760=VECTOR('',#2765,1000.);
#761=VECTOR('',#2768,1000.);
#762=VECTOR('',#2769,1000.);
#763=VECTOR('',#2770,1000.);
#764=VECTOR('',#2777,1000.);
#765=VECTOR('',#2780,1000.);
#766=VECTOR('',#2781,1000.);
#767=VECTOR('',#2782,1000.);
#768=VECTOR('',#2783,1000.);
#769=VECTOR('',#2784,1000.);
#770=VECTOR('',#2785,1000.);
#771=VECTOR('',#2786,1000.);
#772=VECTOR('',#2789,1000.);
#773=VECTOR('',#2790,1000.);
#774=VECTOR('',#2791,1000.);
#775=VECTOR('',#2792,1000.);
#776=VECTOR('',#2799,1000.);
#777=VECTOR('',#2802,1000.);
#778=VECTOR('',#2803,1000.);
#779=VECTOR('',#2806,1000.);
#780=VECTOR('',#2807,1000.);
#781=VECTOR('',#2808,1000.);
#782=VECTOR('',#2809,1000.);
#783=VECTOR('',#2812,1000.);
#784=VECTOR('',#2813,1000.);
#785=VECTOR('',#2814,1000.);
#786=VECTOR('',#2831,1000.);
#787=VECTOR('',#2836,1000.);
#788=VECTOR('',#2837,1000.);
#789=VECTOR('',#2846,1000.);
#790=VECTOR('',#2869,1.25);
#791=VECTOR('',#2876,1.25);
#792=VECTOR('',#2883,1000.);
#793=VECTOR('',#2886,1000.);
#794=VECTOR('',#2891,1000.);
#795=VECTOR('',#2894,1000.);
#796=VECTOR('',#2899,1000.);
#797=VECTOR('',#2902,1000.);
#798=VECTOR('',#2907,1000.);
#799=VECTOR('',#2910,1000.);
#800=VECTOR('',#2913,1000.);
#801=VECTOR('',#2914,1000.);
#802=VECTOR('',#2915,1000.);
#803=VECTOR('',#2918,1000.);
#804=VECTOR('',#2919,1000.);
#805=VECTOR('',#2920,1000.);
#806=VECTOR('',#2923,1000.);
#807=VECTOR('',#2924,1000.);
#808=VECTOR('',#2925,1000.);
#809=VECTOR('',#2928,1000.);
#810=VECTOR('',#2929,1000.);
#811=VECTOR('',#2930,1000.);
#812=VECTOR('',#2933,1000.);
#813=VECTOR('',#2934,1000.);
#814=VECTOR('',#2935,1000.);
#815=VECTOR('',#2938,1000.);
#816=VECTOR('',#2939,1000.);
#817=VECTOR('',#2940,1000.);
#818=VECTOR('',#2943,1000.);
#819=VECTOR('',#2944,1000.);
#820=VECTOR('',#2945,1000.);
#821=VECTOR('',#2946,1000.);
#822=VECTOR('',#2947,1000.);
#823=VECTOR('',#2948,1000.);
#824=VECTOR('',#2949,1000.);
#825=VECTOR('',#2954,1000.);
#826=VECTOR('',#2959,1000.);
#827=VECTOR('',#2960,1000.);
#828=VECTOR('',#2961,1000.);
#829=VECTOR('',#2962,1000.);
#830=VECTOR('',#2965,1000.);
#831=VECTOR('',#2966,1000.);
#832=VECTOR('',#2967,1000.);
#833=VECTOR('',#2970,1000.);
#834=VECTOR('',#2971,1000.);
#835=VECTOR('',#2972,1000.);
#836=VECTOR('',#2975,1000.);
#837=VECTOR('',#2976,1000.);
#838=VECTOR('',#2977,1000.);
#839=VECTOR('',#2980,1000.);
#840=VECTOR('',#2981,1000.);
#841=VECTOR('',#2982,1000.);
#842=VECTOR('',#2985,1000.);
#843=VECTOR('',#2986,1000.);
#844=VECTOR('',#2987,1000.);
#845=VECTOR('',#2990,1000.);
#846=VECTOR('',#2991,1000.);
#847=VECTOR('',#2994,1000.);
#848=VECTOR('',#2995,1000.);
#849=VECTOR('',#2996,1000.);
#850=VECTOR('',#3001,1000.);
#851=VECTOR('',#3004,1000.);
#852=VECTOR('',#3007,1000.);
#853=VECTOR('',#3008,1000.);
#854=VECTOR('',#3009,1000.);
#855=VECTOR('',#3010,1000.);
#856=VECTOR('',#3017,1000.);
#857=VECTOR('',#3018,1000.);
#858=VECTOR('',#3019,1000.);
#859=VECTOR('',#3022,1000.);
#860=VECTOR('',#3023,1000.);
#861=VECTOR('',#3024,1000.);
#862=VECTOR('',#3027,1000.);
#863=VECTOR('',#3028,1000.);
#864=VECTOR('',#3031,1000.);
#865=VECTOR('',#3032,1000.);
#866=VECTOR('',#3043,10.);
#867=VECTOR('',#3044,10.);
#868=VECTOR('',#3053,3.);
#869=VECTOR('',#3060,1.5);
#870=VECTOR('',#3067,2.5);
#871=VECTOR('',#3072,1000.);
#872=VECTOR('',#3075,1000.);
#873=VECTOR('',#3078,1000.);
#874=VECTOR('',#3079,1000.);
#875=VECTOR('',#3080,1000.);
#876=VECTOR('',#3083,1000.);
#877=VECTOR('',#3084,1000.);
#878=VECTOR('',#3085,1000.);
#879=VECTOR('',#3088,1000.);
#880=VECTOR('',#3091,1000.);
#881=VECTOR('',#3108,1.25);
#882=VECTOR('',#3113,1000.);
#883=VECTOR('',#3114,1000.);
#884=VECTOR('',#3115,1000.);
#885=VECTOR('',#3116,1000.);
#886=VECTOR('',#3119,1000.);
#887=VECTOR('',#3120,1000.);
#888=VECTOR('',#3121,1000.);
#889=VECTOR('',#3122,1000.);
#890=VECTOR('',#3125,1000.);
#891=VECTOR('',#3126,1000.);
#892=VECTOR('',#3127,1000.);
#893=VECTOR('',#3128,1000.);
#894=VECTOR('',#3131,1000.);
#895=VECTOR('',#3132,1000.);
#896=VECTOR('',#3133,1000.);
#897=VECTOR('',#3134,1000.);
#898=VECTOR('',#3137,1000.);
#899=VECTOR('',#3138,1000.);
#900=VECTOR('',#3139,1000.);
#901=VECTOR('',#3140,1000.);
#902=VECTOR('',#3143,1000.);
#903=VECTOR('',#3144,1000.);
#904=VECTOR('',#3145,1000.);
#905=VECTOR('',#3146,1000.);
#906=VECTOR('',#3149,1000.);
#907=VECTOR('',#3150,1000.);
#908=VECTOR('',#3151,1000.);
#909=VECTOR('',#3152,1000.);
#910=VECTOR('',#3155,1000.);
#911=VECTOR('',#3156,1000.);
#912=VECTOR('',#3157,1000.);
#913=VECTOR('',#3158,1000.);
#914=VECTOR('',#3161,1000.);
#915=VECTOR('',#3162,1000.);
#916=VECTOR('',#3163,1000.);
#917=VECTOR('',#3164,1000.);
#918=VECTOR('',#3167,1000.);
#919=VECTOR('',#3168,1000.);
#920=VECTOR('',#3169,1000.);
#921=VECTOR('',#3170,1000.);
#922=VECTOR('',#3173,1000.);
#923=VECTOR('',#3174,1000.);
#924=VECTOR('',#3175,1000.);
#925=VECTOR('',#3176,1000.);
#926=VECTOR('',#3179,1000.);
#927=VECTOR('',#3180,1000.);
#928=VECTOR('',#3181,1000.);
#929=VECTOR('',#3184,1000.);
#930=VECTOR('',#3185,1000.);
#931=VECTOR('',#3186,1000.);
#932=VECTOR('',#3189,1000.);
#933=VECTOR('',#3190,1000.);
#934=VECTOR('',#3191,1000.);
#935=VECTOR('',#3192,1000.);
#936=VECTOR('',#3193,1000.);
#937=VECTOR('',#3194,1000.);
#938=VECTOR('',#3195,1000.);
#939=VECTOR('',#3196,1000.);
#940=VECTOR('',#3197,1000.);
#941=VECTOR('',#3198,1000.);
#942=VECTOR('',#3205,1000.);
#943=VECTOR('',#3206,1000.);
#944=VECTOR('',#3207,1000.);
#945=VECTOR('',#3208,1000.);
#946=VECTOR('',#3209,1000.);
#947=VECTOR('',#3210,1000.);
#948=VECTOR('',#3211,1000.);
#949=VECTOR('',#3212,1000.);
#950=VECTOR('',#3213,1000.);
#951=VECTOR('',#3214,1000.);
#952=VECTOR('',#3221,1000.);
#953=VECTOR('',#3226,1000.);
#954=VECTOR('',#3227,1000.);
#955=VECTOR('',#3230,1000.);
#956=VECTOR('',#3233,1000.);
#957=VECTOR('',#3238,1000.);
#958=VECTOR('',#3239,1000.);
#959=VECTOR('',#3242,1000.);
#960=VECTOR('',#3245,1000.);
#961=VECTOR('',#3250,1000.);
#962=VECTOR('',#3251,1000.);
#963=VECTOR('',#3254,1000.);
#964=VECTOR('',#3257,1000.);
#965=VECTOR('',#3262,1000.);
#966=VECTOR('',#3263,1000.);
#967=VECTOR('',#3266,1000.);
#968=VECTOR('',#3269,1000.);
#969=VECTOR('',#3274,1000.);
#970=VECTOR('',#3275,1000.);
#971=VECTOR('',#3278,1000.);
#972=VECTOR('',#3281,1000.);
#973=VECTOR('',#3286,1000.);
#974=VECTOR('',#3287,1000.);
#975=VECTOR('',#3290,1000.);
#976=VECTOR('',#3293,1000.);
#977=VECTOR('',#3298,1000.);
#978=VECTOR('',#3299,1000.);
#979=VECTOR('',#3302,1000.);
#980=VECTOR('',#3305,1000.);
#981=VECTOR('',#3310,1000.);
#982=VECTOR('',#3311,1000.);
#983=VECTOR('',#3314,1000.);
#984=VECTOR('',#3317,1000.);
#985=VECTOR('',#3322,1000.);
#986=VECTOR('',#3323,1000.);
#987=VECTOR('',#3326,1000.);
#988=VECTOR('',#3329,1000.);
#989=VECTOR('',#3334,1000.);
#990=VECTOR('',#3335,1000.);
#991=VECTOR('',#3338,1000.);
#992=VECTOR('',#3341,1000.);
#993=VECTOR('',#3350,1.25);
#994=VECTOR('',#3363,1.5);
#995=CIRCLE('',#2481,1.25);
#996=CIRCLE('',#2482,1.25);
#997=CIRCLE('',#2484,1.25);
#998=CIRCLE('',#2485,1.25);
#999=CIRCLE('',#2487,1.5);
#1000=CIRCLE('',#2488,1.5);
#1001=CIRCLE('',#2490,1.5);
#1002=CIRCLE('',#2491,1.5);
#1003=CIRCLE('',#2493,49.);
#1004=CIRCLE('',#2494,49.);
#1005=CIRCLE('',#2496,44.);
#1006=CIRCLE('',#2497,44.);
#1007=CIRCLE('',#2499,50.);
#1008=CIRCLE('',#2500,50.);
#1009=CIRCLE('',#2502,44.);
#1010=CIRCLE('',#2503,44.);
#1011=CIRCLE('',#2507,4.99999999999999);
#1012=CIRCLE('',#2508,4.99999999999999);
#1013=CIRCLE('',#2512,106.);
#1014=CIRCLE('',#2513,106.);
#1015=CIRCLE('',#2518,4.99999999999999);
#1016=CIRCLE('',#2519,4.99999999999999);
#1017=CIRCLE('',#2521,100.);
#1018=CIRCLE('',#2522,100.);
#1019=CIRCLE('',#2524,106.);
#1020=CIRCLE('',#2525,106.);
#1021=CIRCLE('',#2530,101.);
#1022=CIRCLE('',#2531,101.);
#1023=CIRCLE('',#2533,0.5);
#1024=CIRCLE('',#2535,0.5);
#1025=CIRCLE('',#2541,1.25);
#1026=CIRCLE('',#2542,1.25);
#1027=CIRCLE('',#2544,1.25);
#1028=CIRCLE('',#2545,1.25);
#1029=CIRCLE('',#2547,7.5);
#1030=CIRCLE('',#2548,7.5);
#1031=CIRCLE('',#2550,0.5);
#1032=CIRCLE('',#2551,0.5);
#1033=CIRCLE('',#2553,0.5);
#1034=CIRCLE('',#2554,0.5);
#1035=CIRCLE('',#2556,7.5);
#1036=CIRCLE('',#2557,7.5);
#1037=CIRCLE('',#2566,4.);
#1038=CIRCLE('',#2567,4.);
#1039=CIRCLE('',#2577,4.);
#1040=CIRCLE('',#2581,4.);
#1041=CIRCLE('',#2591,0.500322308738118);
#1042=CIRCLE('',#2592,0.500483076506173);
#1043=CIRCLE('',#2594,3.);
#1044=CIRCLE('',#2595,3.);
#1045=CIRCLE('',#2597,1.5);
#1046=CIRCLE('',#2598,1.5);
#1047=CIRCLE('',#2600,2.5);
#1048=CIRCLE('',#2601,2.5);
#1049=CIRCLE('',#2602,2.5);
#1050=CIRCLE('',#2603,2.5);
#1051=CIRCLE('',#2615,1.25);
#1052=CIRCLE('',#2616,1.25);
#1053=CIRCLE('',#2631,20.5);
#1054=CIRCLE('',#2632,0.5);
#1055=CIRCLE('',#2634,0.5);
#1056=CIRCLE('',#2635,20.5);
#1057=CIRCLE('',#2680,1.25);
#1058=CIRCLE('',#2681,1.25);
#1059=CIRCLE('',#2686,1.5);
#1060=CIRCLE('',#2687,1.5);
#1061=VERTEX_POINT('',#3385);
#1062=VERTEX_POINT('',#3387);
#1063=VERTEX_POINT('',#3391);
#1064=VERTEX_POINT('',#3393);
#1065=VERTEX_POINT('',#3397);
#1066=VERTEX_POINT('',#3399);
#1067=VERTEX_POINT('',#3403);
#1068=VERTEX_POINT('',#3405);
#1069=VERTEX_POINT('',#3409);
#1070=VERTEX_POINT('',#3410);
#1071=VERTEX_POINT('',#3412);
#1072=VERTEX_POINT('',#3414);
#1073=VERTEX_POINT('',#3418);
#1074=VERTEX_POINT('',#3419);
#1075=VERTEX_POINT('',#3421);
#1076=VERTEX_POINT('',#3423);
#1077=VERTEX_POINT('',#3427);
#1078=VERTEX_POINT('',#3428);
#1079=VERTEX_POINT('',#3430);
#1080=VERTEX_POINT('',#3432);
#1081=VERTEX_POINT('',#3436);
#1082=VERTEX_POINT('',#3437);
#1083=VERTEX_POINT('',#3439);
#1084=VERTEX_POINT('',#3441);
#1085=VERTEX_POINT('',#3445);
#1086=VERTEX_POINT('',#3446);
#1087=VERTEX_POINT('',#3448);
#1088=VERTEX_POINT('',#3450);
#1089=VERTEX_POINT('',#3454);
#1090=VERTEX_POINT('',#3456);
#1091=VERTEX_POINT('',#3460);
#1092=VERTEX_POINT('',#3462);
#1093=VERTEX_POINT('',#3466);
#1094=VERTEX_POINT('',#3467);
#1095=VERTEX_POINT('',#3470);
#1096=VERTEX_POINT('',#3472);
#1097=VERTEX_POINT('',#3474);
#1098=VERTEX_POINT('',#3476);
#1099=VERTEX_POINT('',#3485);
#1100=VERTEX_POINT('',#3487);
#1101=VERTEX_POINT('',#3494);
#1102=VERTEX_POINT('',#3495);
#1103=VERTEX_POINT('',#3497);
#1104=VERTEX_POINT('',#3499);
#1105=VERTEX_POINT('',#3503);
#1106=VERTEX_POINT('',#3505);
#1107=VERTEX_POINT('',#3515);
#1108=VERTEX_POINT('',#3517);
#1109=VERTEX_POINT('',#3526);
#1110=VERTEX_POINT('',#3528);
#1111=VERTEX_POINT('',#3540);
#1112=VERTEX_POINT('',#3542);
#1113=VERTEX_POINT('',#3546);
#1114=VERTEX_POINT('',#3548);
#1115=VERTEX_POINT('',#3552);
#1116=VERTEX_POINT('',#3553);
#1117=VERTEX_POINT('',#3555);
#1118=VERTEX_POINT('',#3557);
#1119=VERTEX_POINT('',#3561);
#1120=VERTEX_POINT('',#3562);
#1121=VERTEX_POINT('',#3564);
#1122=VERTEX_POINT('',#3566);
#1123=VERTEX_POINT('',#3570);
#1124=VERTEX_POINT('',#3571);
#1125=VERTEX_POINT('',#3573);
#1126=VERTEX_POINT('',#3575);
#1127=VERTEX_POINT('',#3579);
#1128=VERTEX_POINT('',#3580);
#1129=VERTEX_POINT('',#3582);
#1130=VERTEX_POINT('',#3584);
#1131=VERTEX_POINT('',#3588);
#1132=VERTEX_POINT('',#3590);
#1133=VERTEX_POINT('',#3594);
#1134=VERTEX_POINT('',#3596);
#1135=VERTEX_POINT('',#3600);
#1136=VERTEX_POINT('',#3602);
#1137=VERTEX_POINT('',#3606);
#1138=VERTEX_POINT('',#3608);
#1139=VERTEX_POINT('',#3612);
#1140=VERTEX_POINT('',#3614);
#1141=VERTEX_POINT('',#3618);
#1142=VERTEX_POINT('',#3620);
#1143=VERTEX_POINT('',#3624);
#1144=VERTEX_POINT('',#3626);
#1145=VERTEX_POINT('',#3628);
#1146=VERTEX_POINT('',#3630);
#1147=VERTEX_POINT('',#3632);
#1148=VERTEX_POINT('',#3634);
#1149=VERTEX_POINT('',#3638);
#1150=VERTEX_POINT('',#3640);
#1151=VERTEX_POINT('',#3649);
#1152=VERTEX_POINT('',#3651);
#1153=VERTEX_POINT('',#3655);
#1154=VERTEX_POINT('',#3657);
#1155=VERTEX_POINT('',#3661);
#1156=VERTEX_POINT('',#3663);
#1157=VERTEX_POINT('',#3667);
#1158=VERTEX_POINT('',#3669);
#1159=VERTEX_POINT('',#3673);
#1160=VERTEX_POINT('',#3675);
#1161=VERTEX_POINT('',#3682);
#1162=VERTEX_POINT('',#3684);
#1163=VERTEX_POINT('',#3688);
#1164=VERTEX_POINT('',#3694);
#1165=VERTEX_POINT('',#3695);
#1166=VERTEX_POINT('',#3698);
#1167=VERTEX_POINT('',#3704);
#1168=VERTEX_POINT('',#3706);
#1169=VERTEX_POINT('',#3710);
#1170=VERTEX_POINT('',#3712);
#1171=VERTEX_POINT('',#4014);
#1172=VERTEX_POINT('',#4015);
#1173=VERTEX_POINT('',#4242);
#1174=VERTEX_POINT('',#4244);
#1175=VERTEX_POINT('',#4265);
#1176=VERTEX_POINT('',#5255);
#1177=VERTEX_POINT('',#5256);
#1178=VERTEX_POINT('',#5281);
#1179=VERTEX_POINT('',#7704);
#1180=VERTEX_POINT('',#7706);
#1181=VERTEX_POINT('',#7710);
#1182=VERTEX_POINT('',#7712);
#1183=VERTEX_POINT('',#7716);
#1184=VERTEX_POINT('',#7718);
#1185=VERTEX_POINT('',#7721);
#1186=VERTEX_POINT('',#7722);
#1187=VERTEX_POINT('',#7724);
#1188=VERTEX_POINT('',#7726);
#1189=VERTEX_POINT('',#7730);
#1190=VERTEX_POINT('',#7731);
#1191=VERTEX_POINT('',#7736);
#1192=VERTEX_POINT('',#7738);
#1193=VERTEX_POINT('',#9285);
#1194=VERTEX_POINT('',#9287);
#1195=VERTEX_POINT('',#9291);
#1196=VERTEX_POINT('',#9292);
#1197=VERTEX_POINT('',#9294);
#1198=VERTEX_POINT('',#9296);
#1199=VERTEX_POINT('',#9300);
#1200=VERTEX_POINT('',#9301);
#1201=VERTEX_POINT('',#9303);
#1202=VERTEX_POINT('',#9305);
#1203=VERTEX_POINT('',#9309);
#1204=VERTEX_POINT('',#9310);
#1205=VERTEX_POINT('',#9312);
#1206=VERTEX_POINT('',#9314);
#1207=VERTEX_POINT('',#9318);
#1208=VERTEX_POINT('',#9319);
#1209=VERTEX_POINT('',#9321);
#1210=VERTEX_POINT('',#9323);
#1211=VERTEX_POINT('',#9327);
#1212=VERTEX_POINT('',#9328);
#1213=VERTEX_POINT('',#9330);
#1214=VERTEX_POINT('',#9332);
#1215=VERTEX_POINT('',#9336);
#1216=VERTEX_POINT('',#9337);
#1217=VERTEX_POINT('',#9339);
#1218=VERTEX_POINT('',#9341);
#1219=VERTEX_POINT('',#9345);
#1220=VERTEX_POINT('',#9346);
#1221=VERTEX_POINT('',#9348);
#1222=VERTEX_POINT('',#9350);
#1223=VERTEX_POINT('',#9354);
#1224=VERTEX_POINT('',#9355);
#1225=VERTEX_POINT('',#9357);
#1226=VERTEX_POINT('',#9359);
#1227=VERTEX_POINT('',#9363);
#1228=VERTEX_POINT('',#9364);
#1229=VERTEX_POINT('',#9366);
#1230=VERTEX_POINT('',#9368);
#1231=VERTEX_POINT('',#9372);
#1232=VERTEX_POINT('',#9373);
#1233=VERTEX_POINT('',#9375);
#1234=VERTEX_POINT('',#9377);
#1235=VERTEX_POINT('',#9381);
#1236=VERTEX_POINT('',#9382);
#1237=VERTEX_POINT('',#9384);
#1238=VERTEX_POINT('',#9386);
#1239=VERTEX_POINT('',#9390);
#1240=VERTEX_POINT('',#9392);
#1241=VERTEX_POINT('',#9396);
#1242=VERTEX_POINT('',#9398);
#1243=VERTEX_POINT('',#9412);
#1244=VERTEX_POINT('',#9426);
#1245=VERTEX_POINT('',#9433);
#1246=VERTEX_POINT('',#9442);
#1247=VERTEX_POINT('',#9451);
#1248=VERTEX_POINT('',#9460);
#1249=VERTEX_POINT('',#9469);
#1250=VERTEX_POINT('',#9478);
#1251=VERTEX_POINT('',#9487);
#1252=VERTEX_POINT('',#9496);
#1253=VERTEX_POINT('',#9505);
#1254=VERTEX_POINT('',#9514);
#1255=VERTEX_POINT('',#9524);
#1256=VERTEX_POINT('',#9526);
#1257=VERTEX_POINT('',#9533);
#1258=VERTEX_POINT('',#9535);
#1259=EDGE_CURVE('',#1061,#1061,#995,.T.);
#1260=EDGE_CURVE('',#1061,#1062,#495,.T.);
#1261=EDGE_CURVE('',#1062,#1062,#996,.T.);
#1262=EDGE_CURVE('',#1063,#1063,#997,.T.);
#1263=EDGE_CURVE('',#1063,#1064,#496,.T.);
#1264=EDGE_CURVE('',#1064,#1064,#998,.T.);
#1265=EDGE_CURVE('',#1065,#1065,#999,.T.);
#1266=EDGE_CURVE('',#1065,#1066,#497,.T.);
#1267=EDGE_CURVE('',#1066,#1066,#1000,.T.);
#1268=EDGE_CURVE('',#1067,#1067,#1001,.T.);
#1269=EDGE_CURVE('',#1067,#1068,#498,.T.);
#1270=EDGE_CURVE('',#1068,#1068,#1002,.T.);
#1271=EDGE_CURVE('',#1069,#1070,#1003,.T.);
#1272=EDGE_CURVE('',#1069,#1071,#499,.T.);
#1273=EDGE_CURVE('',#1071,#1072,#1004,.T.);
#1274=EDGE_CURVE('',#1070,#1072,#500,.T.);
#1275=EDGE_CURVE('',#1073,#1074,#1005,.T.);
#1276=EDGE_CURVE('',#1073,#1075,#501,.T.);
#1277=EDGE_CURVE('',#1075,#1076,#1006,.T.);
#1278=EDGE_CURVE('',#1074,#1076,#502,.T.);
#1279=EDGE_CURVE('',#1077,#1078,#1007,.T.);
#1280=EDGE_CURVE('',#1078,#1079,#503,.T.);
#1281=EDGE_CURVE('',#1080,#1079,#1008,.T.);
#1282=EDGE_CURVE('',#1077,#1080,#504,.T.);
#1283=EDGE_CURVE('',#1081,#1082,#1009,.T.);
#1284=EDGE_CURVE('',#1081,#1083,#505,.T.);
#1285=EDGE_CURVE('',#1083,#1084,#1010,.T.);
#1286=EDGE_CURVE('',#1082,#1084,#506,.T.);
#1287=EDGE_CURVE('',#1085,#1086,#507,.T.);
#1288=EDGE_CURVE('',#1085,#1087,#508,.T.);
#1289=EDGE_CURVE('',#1087,#1088,#509,.T.);
#1290=EDGE_CURVE('',#1086,#1088,#510,.T.);
#1291=EDGE_CURVE('',#1086,#1089,#511,.T.);
#1292=EDGE_CURVE('',#1088,#1090,#512,.T.);
#1293=EDGE_CURVE('',#1089,#1090,#513,.T.);
#1294=EDGE_CURVE('',#1089,#1091,#1011,.T.);
#1295=EDGE_CURVE('',#1090,#1092,#1012,.T.);
#1296=EDGE_CURVE('',#1091,#1092,#514,.T.);
#1297=EDGE_CURVE('',#1093,#1094,#515,.T.);
#1298=EDGE_CURVE('',#1094,#1091,#516,.T.);
#1299=EDGE_CURVE('',#1095,#1092,#517,.T.);
#1300=EDGE_CURVE('',#1096,#1095,#518,.T.);
#1301=EDGE_CURVE('',#1096,#1097,#519,.T.);
#1302=EDGE_CURVE('',#1097,#1098,#520,.T.);
#1303=EDGE_CURVE('',#1093,#1098,#521,.T.);
#1304=EDGE_CURVE('',#1071,#1081,#522,.T.);
#1305=EDGE_CURVE('',#1069,#1075,#523,.T.);
#1306=EDGE_CURVE('',#1077,#1073,#524,.T.);
#1307=EDGE_CURVE('',#1080,#1083,#525,.T.);
#1308=EDGE_CURVE('',#1082,#1099,#1013,.T.);
#1309=EDGE_CURVE('',#1084,#1100,#1014,.T.);
#1310=EDGE_CURVE('',#1099,#1100,#526,.T.);
#1311=EDGE_CURVE('',#1099,#1085,#527,.T.);
#1312=EDGE_CURVE('',#1100,#1087,#528,.T.);
#1313=EDGE_CURVE('',#1101,#1102,#529,.T.);
#1314=EDGE_CURVE('',#1102,#1103,#530,.T.);
#1315=EDGE_CURVE('',#1104,#1103,#531,.T.);
#1316=EDGE_CURVE('',#1101,#1104,#532,.T.);
#1317=EDGE_CURVE('',#1103,#1105,#533,.T.);
#1318=EDGE_CURVE('',#1106,#1105,#534,.T.);
#1319=EDGE_CURVE('',#1104,#1106,#535,.T.);
#1320=EDGE_CURVE('',#1105,#1098,#1015,.T.);
#1321=EDGE_CURVE('',#1106,#1097,#1016,.T.);
#1322=EDGE_CURVE('',#1079,#1095,#1017,.T.);
#1323=EDGE_CURVE('',#1078,#1096,#1018,.T.);
#1324=EDGE_CURVE('',#1076,#1107,#1019,.T.);
#1325=EDGE_CURVE('',#1108,#1107,#536,.T.);
#1326=EDGE_CURVE('',#1074,#1108,#1020,.T.);
#1327=EDGE_CURVE('',#1107,#1102,#537,.T.);
#1328=EDGE_CURVE('',#1108,#1101,#538,.T.);
#1329=EDGE_CURVE('',#1072,#1109,#1021,.T.);
#1330=EDGE_CURVE('',#1109,#1110,#539,.T.);
#1331=EDGE_CURVE('',#1070,#1110,#1022,.T.);
#1332=EDGE_CURVE('',#1110,#1093,#1023,.T.);
#1333=EDGE_CURVE('',#1094,#1109,#1024,.T.);
#1334=EDGE_CURVE('',#1111,#1111,#1025,.T.);
#1335=EDGE_CURVE('',#1111,#1112,#540,.T.);
#1336=EDGE_CURVE('',#1112,#1112,#1026,.T.);
#1337=EDGE_CURVE('',#1113,#1113,#1027,.T.);
#1338=EDGE_CURVE('',#1113,#1114,#541,.T.);
#1339=EDGE_CURVE('',#1114,#1114,#1028,.T.);
#1340=EDGE_CURVE('',#1115,#1116,#1029,.T.);
#1341=EDGE_CURVE('',#1115,#1117,#542,.T.);
#1342=EDGE_CURVE('',#1117,#1118,#1030,.T.);
#1343=EDGE_CURVE('',#1116,#1118,#543,.T.);
#1344=EDGE_CURVE('',#1119,#1120,#1031,.T.);
#1345=EDGE_CURVE('',#1121,#1120,#544,.T.);
#1346=EDGE_CURVE('',#1122,#1121,#1032,.T.);
#1347=EDGE_CURVE('',#1119,#1122,#545,.T.);
#1348=EDGE_CURVE('',#1123,#1124,#1033,.T.);
#1349=EDGE_CURVE('',#1125,#1123,#546,.T.);
#1350=EDGE_CURVE('',#1125,#1126,#1034,.T.);
#1351=EDGE_CURVE('',#1124,#1126,#547,.T.);
#1352=EDGE_CURVE('',#1127,#1128,#1035,.T.);
#1353=EDGE_CURVE('',#1127,#1129,#548,.T.);
#1354=EDGE_CURVE('',#1129,#1130,#1036,.T.);
#1355=EDGE_CURVE('',#1128,#1130,#549,.T.);
#1356=EDGE_CURVE('',#1128,#1131,#550,.T.);
#1357=EDGE_CURVE('',#1130,#1132,#551,.T.);
#1358=EDGE_CURVE('',#1131,#1132,#552,.T.);
#1359=EDGE_CURVE('',#1131,#1133,#553,.T.);
#1360=EDGE_CURVE('',#1132,#1134,#554,.T.);
#1361=EDGE_CURVE('',#1133,#1134,#555,.T.);
#1362=EDGE_CURVE('',#1133,#1135,#556,.T.);
#1363=EDGE_CURVE('',#1134,#1136,#557,.T.);
#1364=EDGE_CURVE('',#1135,#1136,#558,.T.);
#1365=EDGE_CURVE('',#1135,#1137,#559,.T.);
#1366=EDGE_CURVE('',#1136,#1138,#560,.T.);
#1367=EDGE_CURVE('',#1137,#1138,#561,.T.);
#1368=EDGE_CURVE('',#1137,#1139,#562,.T.);
#1369=EDGE_CURVE('',#1138,#1140,#563,.T.);
#1370=EDGE_CURVE('',#1139,#1140,#564,.T.);
#1371=EDGE_CURVE('',#1139,#1141,#565,.T.);
#1372=EDGE_CURVE('',#1140,#1142,#566,.T.);
#1373=EDGE_CURVE('',#1141,#1142,#567,.T.);
#1374=EDGE_CURVE('',#1141,#1143,#568,.T.);
#1375=EDGE_CURVE('',#1142,#1144,#569,.T.);
#1376=EDGE_CURVE('',#1145,#1144,#570,.T.);
#1377=EDGE_CURVE('',#1146,#1145,#571,.T.);
#1378=EDGE_CURVE('',#1146,#1147,#572,.T.);
#1379=EDGE_CURVE('',#1147,#1148,#573,.T.);
#1380=EDGE_CURVE('',#1148,#1143,#574,.T.);
#1381=EDGE_CURVE('',#1126,#1149,#1037,.T.);
#1382=EDGE_CURVE('',#1150,#1149,#575,.T.);
#1383=EDGE_CURVE('',#1124,#1150,#1038,.T.);
#1384=EDGE_CURVE('',#1121,#1115,#576,.T.);
#1385=EDGE_CURVE('',#1120,#1125,#577,.T.);
#1386=EDGE_CURVE('',#1123,#1129,#578,.T.);
#1387=EDGE_CURVE('',#1117,#1127,#579,.T.);
#1388=EDGE_CURVE('',#1118,#1151,#580,.T.);
#1389=EDGE_CURVE('',#1152,#1151,#581,.T.);
#1390=EDGE_CURVE('',#1116,#1152,#582,.T.);
#1391=EDGE_CURVE('',#1151,#1153,#583,.T.);
#1392=EDGE_CURVE('',#1154,#1153,#584,.T.);
#1393=EDGE_CURVE('',#1152,#1154,#585,.T.);
#1394=EDGE_CURVE('',#1153,#1155,#586,.T.);
#1395=EDGE_CURVE('',#1156,#1155,#587,.T.);
#1396=EDGE_CURVE('',#1154,#1156,#588,.T.);
#1397=EDGE_CURVE('',#1155,#1157,#589,.T.);
#1398=EDGE_CURVE('',#1158,#1157,#590,.T.);
#1399=EDGE_CURVE('',#1156,#1158,#591,.T.);
#1400=EDGE_CURVE('',#1157,#1159,#592,.T.);
#1401=EDGE_CURVE('',#1160,#1159,#593,.T.);
#1402=EDGE_CURVE('',#1158,#1160,#594,.T.);
#1403=EDGE_CURVE('',#1159,#1147,#595,.T.);
#1404=EDGE_CURVE('',#1160,#1146,#596,.T.);
#1405=EDGE_CURVE('',#1144,#1161,#597,.T.);
#1406=EDGE_CURVE('',#1161,#1162,#598,.T.);
#1407=EDGE_CURVE('',#1145,#1162,#599,.T.);
#1408=EDGE_CURVE('',#1122,#1163,#1039,.T.);
#1409=EDGE_CURVE('',#1163,#1162,#600,.T.);
#1410=EDGE_CURVE('',#1150,#1161,#601,.T.);
#1411=EDGE_CURVE('',#1164,#1165,#602,.T.);
#1412=EDGE_CURVE('',#1164,#1163,#603,.T.);
#1413=EDGE_CURVE('',#1149,#1166,#604,.T.);
#1414=EDGE_CURVE('',#1166,#1165,#605,.T.);
#1415=EDGE_CURVE('',#1119,#1164,#1040,.T.);
#1416=EDGE_CURVE('',#1167,#1120,#606,.T.);
#1417=EDGE_CURVE('',#1167,#1168,#607,.T.);
#1418=EDGE_CURVE('',#1168,#1125,#608,.T.);
#1419=EDGE_CURVE('',#1169,#1127,#609,.T.);
#1420=EDGE_CURVE('',#1170,#1169,#610,.T.);
#1421=EDGE_CURVE('',#1170,#1117,#611,.T.);
#1422=EDGE_CURVE('',#1167,#1170,#612,.T.);
#1423=EDGE_CURVE('',#1168,#1169,#613,.T.);
#1424=EDGE_CURVE('',#1143,#1166,#614,.T.);
#1425=EDGE_CURVE('',#1148,#1165,#615,.T.);
#1426=EDGE_CURVE('',#1171,#1172,#37,.T.);
#1427=EDGE_CURVE('',#1171,#1173,#616,.T.);
#1428=EDGE_CURVE('',#1174,#1173,#38,.T.);
#1429=EDGE_CURVE('',#1175,#1174,#617,.T.);
#1430=EDGE_CURVE('',#1172,#1175,#1041,.T.);
#1431=EDGE_CURVE('',#1176,#1177,#39,.T.);
#1432=EDGE_CURVE('',#1176,#1178,#40,.T.);
#1433=EDGE_CURVE('',#1178,#1171,#1042,.T.);
#1434=EDGE_CURVE('',#1177,#1172,#41,.T.);
#1435=EDGE_CURVE('',#1179,#1179,#1043,.T.);
#1436=EDGE_CURVE('',#1179,#1180,#618,.T.);
#1437=EDGE_CURVE('',#1180,#1180,#1044,.T.);
#1438=EDGE_CURVE('',#1181,#1181,#1045,.T.);
#1439=EDGE_CURVE('',#1181,#1182,#619,.T.);
#1440=EDGE_CURVE('',#1182,#1182,#1046,.T.);
#1441=EDGE_CURVE('',#1183,#1183,#1047,.T.);
#1442=EDGE_CURVE('',#1183,#1184,#620,.T.);
#1443=EDGE_CURVE('',#1184,#1184,#1048,.T.);
#1444=EDGE_CURVE('',#1185,#1186,#1049,.T.);
#1445=EDGE_CURVE('',#1185,#1187,#621,.T.);
#1446=EDGE_CURVE('',#1187,#1188,#1050,.T.);
#1447=EDGE_CURVE('',#1186,#1188,#622,.T.);
#1448=EDGE_CURVE('',#1189,#1190,#623,.T.);
#1449=EDGE_CURVE('',#1186,#1189,#624,.T.);
#1450=EDGE_CURVE('',#1188,#1190,#625,.T.);
#1451=EDGE_CURVE('',#1185,#1191,#626,.T.);
#1452=EDGE_CURVE('',#1191,#1192,#627,.T.);
#1453=EDGE_CURVE('',#1187,#1192,#628,.T.);
#1454=EDGE_CURVE('',#1191,#1189,#629,.T.);
#1455=EDGE_CURVE('',#1192,#1190,#630,.T.);
#1456=EDGE_CURVE('',#1177,#1176,#42,.T.);
#1457=EDGE_CURVE('',#1173,#1174,#43,.T.);
#1458=EDGE_CURVE('',#1175,#1178,#44,.T.);
#1459=EDGE_CURVE('',#1193,#1193,#1051,.T.);
#1460=EDGE_CURVE('',#1193,#1194,#631,.T.);
#1461=EDGE_CURVE('',#1194,#1194,#1052,.T.);
#1462=EDGE_CURVE('',#1195,#1196,#632,.T.);
#1463=EDGE_CURVE('',#1196,#1197,#633,.T.);
#1464=EDGE_CURVE('',#1198,#1197,#634,.T.);
#1465=EDGE_CURVE('',#1195,#1198,#635,.T.);
#1466=EDGE_CURVE('',#1199,#1200,#636,.T.);
#1467=EDGE_CURVE('',#1201,#1199,#637,.T.);
#1468=EDGE_CURVE('',#1201,#1202,#638,.T.);
#1469=EDGE_CURVE('',#1202,#1200,#639,.T.);
#1470=EDGE_CURVE('',#1203,#1204,#640,.T.);
#1471=EDGE_CURVE('',#1205,#1203,#641,.T.);
#1472=EDGE_CURVE('',#1205,#1206,#642,.T.);
#1473=EDGE_CURVE('',#1206,#1204,#643,.T.);
#1474=EDGE_CURVE('',#1207,#1208,#644,.T.);
#1475=EDGE_CURVE('',#1209,#1207,#645,.T.);
#1476=EDGE_CURVE('',#1209,#1210,#646,.T.);
#1477=EDGE_CURVE('',#1210,#1208,#647,.T.);
#1478=EDGE_CURVE('',#1211,#1212,#648,.T.);
#1479=EDGE_CURVE('',#1213,#1211,#649,.T.);
#1480=EDGE_CURVE('',#1213,#1214,#650,.T.);
#1481=EDGE_CURVE('',#1214,#1212,#651,.T.);
#1482=EDGE_CURVE('',#1215,#1216,#652,.T.);
#1483=EDGE_CURVE('',#1217,#1215,#653,.T.);
#1484=EDGE_CURVE('',#1217,#1218,#654,.T.);
#1485=EDGE_CURVE('',#1218,#1216,#655,.T.);
#1486=EDGE_CURVE('',#1219,#1220,#656,.T.);
#1487=EDGE_CURVE('',#1221,#1219,#657,.T.);
#1488=EDGE_CURVE('',#1221,#1222,#658,.T.);
#1489=EDGE_CURVE('',#1222,#1220,#659,.T.);
#1490=EDGE_CURVE('',#1223,#1224,#660,.T.);
#1491=EDGE_CURVE('',#1225,#1223,#661,.T.);
#1492=EDGE_CURVE('',#1225,#1226,#662,.T.);
#1493=EDGE_CURVE('',#1226,#1224,#663,.T.);
#1494=EDGE_CURVE('',#1227,#1228,#664,.T.);
#1495=EDGE_CURVE('',#1229,#1227,#665,.T.);
#1496=EDGE_CURVE('',#1229,#1230,#666,.T.);
#1497=EDGE_CURVE('',#1230,#1228,#667,.T.);
#1498=EDGE_CURVE('',#1231,#1232,#668,.T.);
#1499=EDGE_CURVE('',#1231,#1233,#669,.T.);
#1500=EDGE_CURVE('',#1233,#1234,#670,.T.);
#1501=EDGE_CURVE('',#1234,#1232,#671,.T.);
#1502=EDGE_CURVE('',#1235,#1236,#672,.T.);
#1503=EDGE_CURVE('',#1237,#1235,#673,.T.);
#1504=EDGE_CURVE('',#1238,#1237,#674,.T.);
#1505=EDGE_CURVE('',#1238,#1236,#675,.T.);
#1506=EDGE_CURVE('',#1239,#1237,#676,.T.);
#1507=EDGE_CURVE('',#1240,#1239,#677,.T.);
#1508=EDGE_CURVE('',#1240,#1238,#678,.T.);
#1509=EDGE_CURVE('',#1239,#1241,#679,.T.);
#1510=EDGE_CURVE('',#1241,#1242,#680,.T.);
#1511=EDGE_CURVE('',#1240,#1242,#681,.T.);
#1512=EDGE_CURVE('',#1233,#1197,#682,.T.);
#1513=EDGE_CURVE('',#1196,#1200,#683,.T.);
#1514=EDGE_CURVE('',#1202,#1204,#684,.T.);
#1515=EDGE_CURVE('',#1206,#1208,#685,.T.);
#1516=EDGE_CURVE('',#1210,#1212,#686,.T.);
#1517=EDGE_CURVE('',#1214,#1216,#687,.T.);
#1518=EDGE_CURVE('',#1218,#1220,#688,.T.);
#1519=EDGE_CURVE('',#1222,#1224,#689,.T.);
#1520=EDGE_CURVE('',#1226,#1228,#690,.T.);
#1521=EDGE_CURVE('',#1230,#1236,#691,.T.);
#1522=EDGE_CURVE('',#1242,#1243,#1053,.T.);
#1523=EDGE_CURVE('',#1243,#1234,#1054,.T.);
#1524=EDGE_CURVE('',#1235,#1229,#692,.T.);
#1525=EDGE_CURVE('',#1227,#1225,#693,.T.);
#1526=EDGE_CURVE('',#1223,#1221,#694,.T.);
#1527=EDGE_CURVE('',#1219,#1217,#695,.T.);
#1528=EDGE_CURVE('',#1215,#1213,#696,.T.);
#1529=EDGE_CURVE('',#1211,#1209,#697,.T.);
#1530=EDGE_CURVE('',#1207,#1205,#698,.T.);
#1531=EDGE_CURVE('',#1203,#1201,#699,.T.);
#1532=EDGE_CURVE('',#1199,#1195,#700,.T.);
#1533=EDGE_CURVE('',#1198,#1231,#701,.T.);
#1534=EDGE_CURVE('',#1232,#1244,#1055,.T.);
#1535=EDGE_CURVE('',#1244,#1241,#1056,.T.);
#1536=EDGE_CURVE('',#1244,#1243,#702,.T.);
#1537=EDGE_CURVE('',#1231,#1245,#703,.T.);
#1538=EDGE_CURVE('',#1245,#1233,#704,.T.);
#1539=EDGE_CURVE('',#1197,#1245,#705,.T.);
#1540=EDGE_CURVE('',#1198,#1245,#706,.T.);
#1541=EDGE_CURVE('',#1229,#1246,#707,.T.);
#1542=EDGE_CURVE('',#1246,#1230,#708,.T.);
#1543=EDGE_CURVE('',#1236,#1246,#709,.T.);
#1544=EDGE_CURVE('',#1235,#1246,#710,.T.);
#1545=EDGE_CURVE('',#1225,#1247,#711,.T.);
#1546=EDGE_CURVE('',#1247,#1226,#712,.T.);
#1547=EDGE_CURVE('',#1228,#1247,#713,.T.);
#1548=EDGE_CURVE('',#1227,#1247,#714,.T.);
#1549=EDGE_CURVE('',#1221,#1248,#715,.T.);
#1550=EDGE_CURVE('',#1248,#1222,#716,.T.);
#1551=EDGE_CURVE('',#1224,#1248,#717,.T.);
#1552=EDGE_CURVE('',#1223,#1248,#718,.T.);
#1553=EDGE_CURVE('',#1217,#1249,#719,.T.);
#1554=EDGE_CURVE('',#1249,#1218,#720,.T.);
#1555=EDGE_CURVE('',#1220,#1249,#721,.T.);
#1556=EDGE_CURVE('',#1219,#1249,#722,.T.);
#1557=EDGE_CURVE('',#1213,#1250,#723,.T.);
#1558=EDGE_CURVE('',#1250,#1214,#724,.T.);
#1559=EDGE_CURVE('',#1216,#1250,#725,.T.);
#1560=EDGE_CURVE('',#1215,#1250,#726,.T.);
#1561=EDGE_CURVE('',#1209,#1251,#727,.T.);
#1562=EDGE_CURVE('',#1251,#1210,#728,.T.);
#1563=EDGE_CURVE('',#1212,#1251,#729,.T.);
#1564=EDGE_CURVE('',#1211,#1251,#730,.T.);
#1565=EDGE_CURVE('',#1205,#1252,#731,.T.);
#1566=EDGE_CURVE('',#1252,#1206,#732,.T.);
#1567=EDGE_CURVE('',#1208,#1252,#733,.T.);
#1568=EDGE_CURVE('',#1207,#1252,#734,.T.);
#1569=EDGE_CURVE('',#1201,#1253,#735,.T.);
#1570=EDGE_CURVE('',#1253,#1202,#736,.T.);
#1571=EDGE_CURVE('',#1204,#1253,#737,.T.);
#1572=EDGE_CURVE('',#1203,#1253,#738,.T.);
#1573=EDGE_CURVE('',#1195,#1254,#739,.T.);
#1574=EDGE_CURVE('',#1254,#1196,#740,.T.);
#1575=EDGE_CURVE('',#1200,#1254,#741,.T.);
#1576=EDGE_CURVE('',#1199,#1254,#742,.T.);
#1577=EDGE_CURVE('',#1255,#1255,#1057,.T.);
#1578=EDGE_CURVE('',#1255,#1256,#743,.T.);
#1579=EDGE_CURVE('',#1256,#1256,#1058,.T.);
#1580=EDGE_CURVE('',#1257,#1257,#1059,.T.);
#1581=EDGE_CURVE('',#1257,#1258,#744,.T.);
#1582=EDGE_CURVE('',#1258,#1258,#1060,.T.);
#1583=ORIENTED_EDGE('',*,*,#1259,.F.);
#1584=ORIENTED_EDGE('',*,*,#1260,.T.);
#1585=ORIENTED_EDGE('',*,*,#1261,.T.);
#1586=ORIENTED_EDGE('',*,*,#1260,.F.);
#1587=ORIENTED_EDGE('',*,*,#1262,.F.);
#1588=ORIENTED_EDGE('',*,*,#1263,.T.);
#1589=ORIENTED_EDGE('',*,*,#1264,.T.);
#1590=ORIENTED_EDGE('',*,*,#1263,.F.);
#1591=ORIENTED_EDGE('',*,*,#1265,.F.);
#1592=ORIENTED_EDGE('',*,*,#1266,.T.);
#1593=ORIENTED_EDGE('',*,*,#1267,.T.);
#1594=ORIENTED_EDGE('',*,*,#1266,.F.);
#1595=ORIENTED_EDGE('',*,*,#1268,.F.);
#1596=ORIENTED_EDGE('',*,*,#1269,.T.);
#1597=ORIENTED_EDGE('',*,*,#1270,.T.);
#1598=ORIENTED_EDGE('',*,*,#1269,.F.);
#1599=ORIENTED_EDGE('',*,*,#1271,.F.);
#1600=ORIENTED_EDGE('',*,*,#1272,.T.);
#1601=ORIENTED_EDGE('',*,*,#1273,.T.);
#1602=ORIENTED_EDGE('',*,*,#1274,.F.);
#1603=ORIENTED_EDGE('',*,*,#1275,.F.);
#1604=ORIENTED_EDGE('',*,*,#1276,.T.);
#1605=ORIENTED_EDGE('',*,*,#1277,.T.);
#1606=ORIENTED_EDGE('',*,*,#1278,.F.);
#1607=ORIENTED_EDGE('',*,*,#1279,.T.);
#1608=ORIENTED_EDGE('',*,*,#1280,.T.);
#1609=ORIENTED_EDGE('',*,*,#1281,.F.);
#1610=ORIENTED_EDGE('',*,*,#1282,.F.);
#1611=ORIENTED_EDGE('',*,*,#1283,.F.);
#1612=ORIENTED_EDGE('',*,*,#1284,.T.);
#1613=ORIENTED_EDGE('',*,*,#1285,.T.);
#1614=ORIENTED_EDGE('',*,*,#1286,.F.);
#1615=ORIENTED_EDGE('',*,*,#1287,.F.);
#1616=ORIENTED_EDGE('',*,*,#1288,.T.);
#1617=ORIENTED_EDGE('',*,*,#1289,.T.);
#1618=ORIENTED_EDGE('',*,*,#1290,.F.);
#1619=ORIENTED_EDGE('',*,*,#1291,.F.);
#1620=ORIENTED_EDGE('',*,*,#1290,.T.);
#1621=ORIENTED_EDGE('',*,*,#1292,.T.);
#1622=ORIENTED_EDGE('',*,*,#1293,.F.);
#1623=ORIENTED_EDGE('',*,*,#1294,.F.);
#1624=ORIENTED_EDGE('',*,*,#1293,.T.);
#1625=ORIENTED_EDGE('',*,*,#1295,.T.);
#1626=ORIENTED_EDGE('',*,*,#1296,.F.);
#1627=ORIENTED_EDGE('',*,*,#1297,.T.);
#1628=ORIENTED_EDGE('',*,*,#1298,.T.);
#1629=ORIENTED_EDGE('',*,*,#1296,.T.);
#1630=ORIENTED_EDGE('',*,*,#1299,.F.);
#1631=ORIENTED_EDGE('',*,*,#1300,.F.);
#1632=ORIENTED_EDGE('',*,*,#1301,.T.);
#1633=ORIENTED_EDGE('',*,*,#1302,.T.);
#1634=ORIENTED_EDGE('',*,*,#1303,.F.);
#1635=ORIENTED_EDGE('',*,*,#1304,.F.);
#1636=ORIENTED_EDGE('',*,*,#1272,.F.);
#1637=ORIENTED_EDGE('',*,*,#1305,.T.);
#1638=ORIENTED_EDGE('',*,*,#1276,.F.);
#1639=ORIENTED_EDGE('',*,*,#1306,.F.);
#1640=ORIENTED_EDGE('',*,*,#1282,.T.);
#1641=ORIENTED_EDGE('',*,*,#1307,.T.);
#1642=ORIENTED_EDGE('',*,*,#1284,.F.);
#1643=ORIENTED_EDGE('',*,*,#1308,.F.);
#1644=ORIENTED_EDGE('',*,*,#1286,.T.);
#1645=ORIENTED_EDGE('',*,*,#1309,.T.);
#1646=ORIENTED_EDGE('',*,*,#1310,.F.);
#1647=ORIENTED_EDGE('',*,*,#1311,.F.);
#1648=ORIENTED_EDGE('',*,*,#1310,.T.);
#1649=ORIENTED_EDGE('',*,*,#1312,.T.);
#1650=ORIENTED_EDGE('',*,*,#1288,.F.);
#1651=ORIENTED_EDGE('',*,*,#1313,.T.);
#1652=ORIENTED_EDGE('',*,*,#1314,.T.);
#1653=ORIENTED_EDGE('',*,*,#1315,.F.);
#1654=ORIENTED_EDGE('',*,*,#1316,.F.);
#1655=ORIENTED_EDGE('',*,*,#1315,.T.);
#1656=ORIENTED_EDGE('',*,*,#1317,.T.);
#1657=ORIENTED_EDGE('',*,*,#1318,.F.);
#1658=ORIENTED_EDGE('',*,*,#1319,.F.);
#1659=ORIENTED_EDGE('',*,*,#1318,.T.);
#1660=ORIENTED_EDGE('',*,*,#1320,.T.);
#1661=ORIENTED_EDGE('',*,*,#1302,.F.);
#1662=ORIENTED_EDGE('',*,*,#1321,.F.);
#1663=ORIENTED_EDGE('',*,*,#1322,.F.);
#1664=ORIENTED_EDGE('',*,*,#1280,.F.);
#1665=ORIENTED_EDGE('',*,*,#1323,.T.);
#1666=ORIENTED_EDGE('',*,*,#1300,.T.);
#1667=ORIENTED_EDGE('',*,*,#1278,.T.);
#1668=ORIENTED_EDGE('',*,*,#1324,.T.);
#1669=ORIENTED_EDGE('',*,*,#1325,.F.);
#1670=ORIENTED_EDGE('',*,*,#1326,.F.);
#1671=ORIENTED_EDGE('',*,*,#1325,.T.);
#1672=ORIENTED_EDGE('',*,*,#1327,.T.);
#1673=ORIENTED_EDGE('',*,*,#1313,.F.);
#1674=ORIENTED_EDGE('',*,*,#1328,.F.);
#1675=ORIENTED_EDGE('',*,*,#1316,.T.);
#1676=ORIENTED_EDGE('',*,*,#1319,.T.);
#1677=ORIENTED_EDGE('',*,*,#1321,.T.);
#1678=ORIENTED_EDGE('',*,*,#1301,.F.);
#1679=ORIENTED_EDGE('',*,*,#1323,.F.);
#1680=ORIENTED_EDGE('',*,*,#1279,.F.);
#1681=ORIENTED_EDGE('',*,*,#1306,.T.);
#1682=ORIENTED_EDGE('',*,*,#1275,.T.);
#1683=ORIENTED_EDGE('',*,*,#1326,.T.);
#1684=ORIENTED_EDGE('',*,*,#1328,.T.);
#1685=ORIENTED_EDGE('',*,*,#1261,.F.);
#1686=ORIENTED_EDGE('',*,*,#1289,.F.);
#1687=ORIENTED_EDGE('',*,*,#1312,.F.);
#1688=ORIENTED_EDGE('',*,*,#1309,.F.);
#1689=ORIENTED_EDGE('',*,*,#1285,.F.);
#1690=ORIENTED_EDGE('',*,*,#1307,.F.);
#1691=ORIENTED_EDGE('',*,*,#1281,.T.);
#1692=ORIENTED_EDGE('',*,*,#1322,.T.);
#1693=ORIENTED_EDGE('',*,*,#1299,.T.);
#1694=ORIENTED_EDGE('',*,*,#1295,.F.);
#1695=ORIENTED_EDGE('',*,*,#1292,.F.);
#1696=ORIENTED_EDGE('',*,*,#1262,.T.);
#1697=ORIENTED_EDGE('',*,*,#1329,.T.);
#1698=ORIENTED_EDGE('',*,*,#1330,.T.);
#1699=ORIENTED_EDGE('',*,*,#1331,.F.);
#1700=ORIENTED_EDGE('',*,*,#1274,.T.);
#1701=ORIENTED_EDGE('',*,*,#1314,.F.);
#1702=ORIENTED_EDGE('',*,*,#1327,.F.);
#1703=ORIENTED_EDGE('',*,*,#1324,.F.);
#1704=ORIENTED_EDGE('',*,*,#1277,.F.);
#1705=ORIENTED_EDGE('',*,*,#1305,.F.);
#1706=ORIENTED_EDGE('',*,*,#1271,.T.);
#1707=ORIENTED_EDGE('',*,*,#1331,.T.);
#1708=ORIENTED_EDGE('',*,*,#1332,.T.);
#1709=ORIENTED_EDGE('',*,*,#1303,.T.);
#1710=ORIENTED_EDGE('',*,*,#1320,.F.);
#1711=ORIENTED_EDGE('',*,*,#1317,.F.);
#1712=ORIENTED_EDGE('',*,*,#1259,.T.);
#1713=ORIENTED_EDGE('',*,*,#1265,.T.);
#1714=ORIENTED_EDGE('',*,*,#1287,.T.);
#1715=ORIENTED_EDGE('',*,*,#1291,.T.);
#1716=ORIENTED_EDGE('',*,*,#1294,.T.);
#1717=ORIENTED_EDGE('',*,*,#1298,.F.);
#1718=ORIENTED_EDGE('',*,*,#1333,.T.);
#1719=ORIENTED_EDGE('',*,*,#1329,.F.);
#1720=ORIENTED_EDGE('',*,*,#1273,.F.);
#1721=ORIENTED_EDGE('',*,*,#1304,.T.);
#1722=ORIENTED_EDGE('',*,*,#1283,.T.);
#1723=ORIENTED_EDGE('',*,*,#1308,.T.);
#1724=ORIENTED_EDGE('',*,*,#1311,.T.);
#1725=ORIENTED_EDGE('',*,*,#1264,.F.);
#1726=ORIENTED_EDGE('',*,*,#1270,.F.);
#1727=ORIENTED_EDGE('',*,*,#1332,.F.);
#1728=ORIENTED_EDGE('',*,*,#1330,.F.);
#1729=ORIENTED_EDGE('',*,*,#1333,.F.);
#1730=ORIENTED_EDGE('',*,*,#1297,.F.);
#1731=ORIENTED_EDGE('',*,*,#1268,.T.);
#1732=ORIENTED_EDGE('',*,*,#1267,.F.);
#1733=ORIENTED_EDGE('',*,*,#1334,.T.);
#1734=ORIENTED_EDGE('',*,*,#1335,.T.);
#1735=ORIENTED_EDGE('',*,*,#1336,.T.);
#1736=ORIENTED_EDGE('',*,*,#1335,.F.);
#1737=ORIENTED_EDGE('',*,*,#1337,.F.);
#1738=ORIENTED_EDGE('',*,*,#1338,.T.);
#1739=ORIENTED_EDGE('',*,*,#1339,.F.);
#1740=ORIENTED_EDGE('',*,*,#1338,.F.);
#1741=ORIENTED_EDGE('',*,*,#1340,.F.);
#1742=ORIENTED_EDGE('',*,*,#1341,.T.);
#1743=ORIENTED_EDGE('',*,*,#1342,.T.);
#1744=ORIENTED_EDGE('',*,*,#1343,.F.);
#1745=ORIENTED_EDGE('',*,*,#1344,.T.);
#1746=ORIENTED_EDGE('',*,*,#1345,.F.);
#1747=ORIENTED_EDGE('',*,*,#1346,.F.);
#1748=ORIENTED_EDGE('',*,*,#1347,.F.);
#1749=ORIENTED_EDGE('',*,*,#1348,.F.);
#1750=ORIENTED_EDGE('',*,*,#1349,.F.);
#1751=ORIENTED_EDGE('',*,*,#1350,.T.);
#1752=ORIENTED_EDGE('',*,*,#1351,.F.);
#1753=ORIENTED_EDGE('',*,*,#1352,.F.);
#1754=ORIENTED_EDGE('',*,*,#1353,.T.);
#1755=ORIENTED_EDGE('',*,*,#1354,.T.);
#1756=ORIENTED_EDGE('',*,*,#1355,.F.);
#1757=ORIENTED_EDGE('',*,*,#1356,.F.);
#1758=ORIENTED_EDGE('',*,*,#1355,.T.);
#1759=ORIENTED_EDGE('',*,*,#1357,.T.);
#1760=ORIENTED_EDGE('',*,*,#1358,.F.);
#1761=ORIENTED_EDGE('',*,*,#1359,.F.);
#1762=ORIENTED_EDGE('',*,*,#1358,.T.);
#1763=ORIENTED_EDGE('',*,*,#1360,.T.);
#1764=ORIENTED_EDGE('',*,*,#1361,.F.);
#1765=ORIENTED_EDGE('',*,*,#1362,.F.);
#1766=ORIENTED_EDGE('',*,*,#1361,.T.);
#1767=ORIENTED_EDGE('',*,*,#1363,.T.);
#1768=ORIENTED_EDGE('',*,*,#1364,.F.);
#1769=ORIENTED_EDGE('',*,*,#1365,.F.);
#1770=ORIENTED_EDGE('',*,*,#1364,.T.);
#1771=ORIENTED_EDGE('',*,*,#1366,.T.);
#1772=ORIENTED_EDGE('',*,*,#1367,.F.);
#1773=ORIENTED_EDGE('',*,*,#1368,.F.);
#1774=ORIENTED_EDGE('',*,*,#1367,.T.);
#1775=ORIENTED_EDGE('',*,*,#1369,.T.);
#1776=ORIENTED_EDGE('',*,*,#1370,.F.);
#1777=ORIENTED_EDGE('',*,*,#1371,.F.);
#1778=ORIENTED_EDGE('',*,*,#1370,.T.);
#1779=ORIENTED_EDGE('',*,*,#1372,.T.);
#1780=ORIENTED_EDGE('',*,*,#1373,.F.);
#1781=ORIENTED_EDGE('',*,*,#1374,.F.);
#1782=ORIENTED_EDGE('',*,*,#1373,.T.);
#1783=ORIENTED_EDGE('',*,*,#1375,.T.);
#1784=ORIENTED_EDGE('',*,*,#1376,.F.);
#1785=ORIENTED_EDGE('',*,*,#1377,.F.);
#1786=ORIENTED_EDGE('',*,*,#1378,.T.);
#1787=ORIENTED_EDGE('',*,*,#1379,.T.);
#1788=ORIENTED_EDGE('',*,*,#1380,.T.);
#1789=ORIENTED_EDGE('',*,*,#1351,.T.);
#1790=ORIENTED_EDGE('',*,*,#1381,.T.);
#1791=ORIENTED_EDGE('',*,*,#1382,.F.);
#1792=ORIENTED_EDGE('',*,*,#1383,.F.);
#1793=ORIENTED_EDGE('',*,*,#1384,.F.);
#1794=ORIENTED_EDGE('',*,*,#1345,.T.);
#1795=ORIENTED_EDGE('',*,*,#1385,.T.);
#1796=ORIENTED_EDGE('',*,*,#1349,.T.);
#1797=ORIENTED_EDGE('',*,*,#1386,.T.);
#1798=ORIENTED_EDGE('',*,*,#1353,.F.);
#1799=ORIENTED_EDGE('',*,*,#1387,.F.);
#1800=ORIENTED_EDGE('',*,*,#1341,.F.);
#1801=ORIENTED_EDGE('',*,*,#1343,.T.);
#1802=ORIENTED_EDGE('',*,*,#1388,.T.);
#1803=ORIENTED_EDGE('',*,*,#1389,.F.);
#1804=ORIENTED_EDGE('',*,*,#1390,.F.);
#1805=ORIENTED_EDGE('',*,*,#1389,.T.);
#1806=ORIENTED_EDGE('',*,*,#1391,.T.);
#1807=ORIENTED_EDGE('',*,*,#1392,.F.);
#1808=ORIENTED_EDGE('',*,*,#1393,.F.);
#1809=ORIENTED_EDGE('',*,*,#1392,.T.);
#1810=ORIENTED_EDGE('',*,*,#1394,.T.);
#1811=ORIENTED_EDGE('',*,*,#1395,.F.);
#1812=ORIENTED_EDGE('',*,*,#1396,.F.);
#1813=ORIENTED_EDGE('',*,*,#1395,.T.);
#1814=ORIENTED_EDGE('',*,*,#1397,.T.);
#1815=ORIENTED_EDGE('',*,*,#1398,.F.);
#1816=ORIENTED_EDGE('',*,*,#1399,.F.);
#1817=ORIENTED_EDGE('',*,*,#1398,.T.);
#1818=ORIENTED_EDGE('',*,*,#1400,.T.);
#1819=ORIENTED_EDGE('',*,*,#1401,.F.);
#1820=ORIENTED_EDGE('',*,*,#1402,.F.);
#1821=ORIENTED_EDGE('',*,*,#1401,.T.);
#1822=ORIENTED_EDGE('',*,*,#1403,.T.);
#1823=ORIENTED_EDGE('',*,*,#1378,.F.);
#1824=ORIENTED_EDGE('',*,*,#1404,.F.);
#1825=ORIENTED_EDGE('',*,*,#1405,.T.);
#1826=ORIENTED_EDGE('',*,*,#1406,.T.);
#1827=ORIENTED_EDGE('',*,*,#1407,.F.);
#1828=ORIENTED_EDGE('',*,*,#1376,.T.);
#1829=ORIENTED_EDGE('',*,*,#1408,.F.);
#1830=ORIENTED_EDGE('',*,*,#1346,.T.);
#1831=ORIENTED_EDGE('',*,*,#1384,.T.);
#1832=ORIENTED_EDGE('',*,*,#1340,.T.);
#1833=ORIENTED_EDGE('',*,*,#1390,.T.);
#1834=ORIENTED_EDGE('',*,*,#1393,.T.);
#1835=ORIENTED_EDGE('',*,*,#1396,.T.);
#1836=ORIENTED_EDGE('',*,*,#1399,.T.);
#1837=ORIENTED_EDGE('',*,*,#1402,.T.);
#1838=ORIENTED_EDGE('',*,*,#1404,.T.);
#1839=ORIENTED_EDGE('',*,*,#1377,.T.);
#1840=ORIENTED_EDGE('',*,*,#1407,.T.);
#1841=ORIENTED_EDGE('',*,*,#1409,.F.);
#1842=ORIENTED_EDGE('',*,*,#1386,.F.);
#1843=ORIENTED_EDGE('',*,*,#1348,.T.);
#1844=ORIENTED_EDGE('',*,*,#1383,.T.);
#1845=ORIENTED_EDGE('',*,*,#1410,.T.);
#1846=ORIENTED_EDGE('',*,*,#1405,.F.);
#1847=ORIENTED_EDGE('',*,*,#1375,.F.);
#1848=ORIENTED_EDGE('',*,*,#1372,.F.);
#1849=ORIENTED_EDGE('',*,*,#1369,.F.);
#1850=ORIENTED_EDGE('',*,*,#1366,.F.);
#1851=ORIENTED_EDGE('',*,*,#1363,.F.);
#1852=ORIENTED_EDGE('',*,*,#1360,.F.);
#1853=ORIENTED_EDGE('',*,*,#1357,.F.);
#1854=ORIENTED_EDGE('',*,*,#1354,.F.);
#1855=ORIENTED_EDGE('',*,*,#1411,.F.);
#1856=ORIENTED_EDGE('',*,*,#1412,.T.);
#1857=ORIENTED_EDGE('',*,*,#1409,.T.);
#1858=ORIENTED_EDGE('',*,*,#1406,.F.);
#1859=ORIENTED_EDGE('',*,*,#1410,.F.);
#1860=ORIENTED_EDGE('',*,*,#1382,.T.);
#1861=ORIENTED_EDGE('',*,*,#1413,.T.);
#1862=ORIENTED_EDGE('',*,*,#1414,.T.);
#1863=ORIENTED_EDGE('',*,*,#1415,.F.);
#1864=ORIENTED_EDGE('',*,*,#1347,.T.);
#1865=ORIENTED_EDGE('',*,*,#1408,.T.);
#1866=ORIENTED_EDGE('',*,*,#1412,.F.);
#1867=ORIENTED_EDGE('',*,*,#1385,.F.);
#1868=ORIENTED_EDGE('',*,*,#1416,.F.);
#1869=ORIENTED_EDGE('',*,*,#1417,.T.);
#1870=ORIENTED_EDGE('',*,*,#1418,.T.);
#1871=ORIENTED_EDGE('',*,*,#1387,.T.);
#1872=ORIENTED_EDGE('',*,*,#1419,.F.);
#1873=ORIENTED_EDGE('',*,*,#1420,.F.);
#1874=ORIENTED_EDGE('',*,*,#1421,.T.);
#1875=ORIENTED_EDGE('',*,*,#1422,.T.);
#1876=ORIENTED_EDGE('',*,*,#1420,.T.);
#1877=ORIENTED_EDGE('',*,*,#1423,.F.);
#1878=ORIENTED_EDGE('',*,*,#1417,.F.);
#1879=ORIENTED_EDGE('',*,*,#1424,.F.);
#1880=ORIENTED_EDGE('',*,*,#1380,.F.);
#1881=ORIENTED_EDGE('',*,*,#1425,.T.);
#1882=ORIENTED_EDGE('',*,*,#1414,.F.);
#1883=ORIENTED_EDGE('',*,*,#1415,.T.);
#1884=ORIENTED_EDGE('',*,*,#1411,.T.);
#1885=ORIENTED_EDGE('',*,*,#1425,.F.);
#1886=ORIENTED_EDGE('',*,*,#1379,.F.);
#1887=ORIENTED_EDGE('',*,*,#1403,.F.);
#1888=ORIENTED_EDGE('',*,*,#1400,.F.);
#1889=ORIENTED_EDGE('',*,*,#1397,.F.);
#1890=ORIENTED_EDGE('',*,*,#1394,.F.);
#1891=ORIENTED_EDGE('',*,*,#1391,.F.);
#1892=ORIENTED_EDGE('',*,*,#1388,.F.);
#1893=ORIENTED_EDGE('',*,*,#1342,.F.);
#1894=ORIENTED_EDGE('',*,*,#1421,.F.);
#1895=ORIENTED_EDGE('',*,*,#1422,.F.);
#1896=ORIENTED_EDGE('',*,*,#1416,.T.);
#1897=ORIENTED_EDGE('',*,*,#1344,.F.);
#1898=ORIENTED_EDGE('',*,*,#1334,.F.);
#1899=ORIENTED_EDGE('',*,*,#1423,.T.);
#1900=ORIENTED_EDGE('',*,*,#1419,.T.);
#1901=ORIENTED_EDGE('',*,*,#1352,.T.);
#1902=ORIENTED_EDGE('',*,*,#1356,.T.);
#1903=ORIENTED_EDGE('',*,*,#1359,.T.);
#1904=ORIENTED_EDGE('',*,*,#1362,.T.);
#1905=ORIENTED_EDGE('',*,*,#1365,.T.);
#1906=ORIENTED_EDGE('',*,*,#1368,.T.);
#1907=ORIENTED_EDGE('',*,*,#1371,.T.);
#1908=ORIENTED_EDGE('',*,*,#1374,.T.);
#1909=ORIENTED_EDGE('',*,*,#1424,.T.);
#1910=ORIENTED_EDGE('',*,*,#1413,.F.);
#1911=ORIENTED_EDGE('',*,*,#1381,.F.);
#1912=ORIENTED_EDGE('',*,*,#1350,.F.);
#1913=ORIENTED_EDGE('',*,*,#1418,.F.);
#1914=ORIENTED_EDGE('',*,*,#1339,.T.);
#1915=ORIENTED_EDGE('',*,*,#1337,.T.);
#1916=ORIENTED_EDGE('',*,*,#1336,.F.);
#1917=ORIENTED_EDGE('',*,*,#1426,.F.);
#1918=ORIENTED_EDGE('',*,*,#1427,.T.);
#1919=ORIENTED_EDGE('',*,*,#1428,.F.);
#1920=ORIENTED_EDGE('',*,*,#1429,.F.);
#1921=ORIENTED_EDGE('',*,*,#1430,.F.);
#1922=ORIENTED_EDGE('',*,*,#1431,.F.);
#1923=ORIENTED_EDGE('',*,*,#1432,.T.);
#1924=ORIENTED_EDGE('',*,*,#1433,.T.);
#1925=ORIENTED_EDGE('',*,*,#1426,.T.);
#1926=ORIENTED_EDGE('',*,*,#1434,.F.);
#1927=ORIENTED_EDGE('',*,*,#1435,.T.);
#1928=ORIENTED_EDGE('',*,*,#1436,.T.);
#1929=ORIENTED_EDGE('',*,*,#1437,.F.);
#1930=ORIENTED_EDGE('',*,*,#1436,.F.);
#1931=ORIENTED_EDGE('',*,*,#1438,.T.);
#1932=ORIENTED_EDGE('',*,*,#1439,.T.);
#1933=ORIENTED_EDGE('',*,*,#1440,.F.);
#1934=ORIENTED_EDGE('',*,*,#1439,.F.);
#1935=ORIENTED_EDGE('',*,*,#1441,.T.);
#1936=ORIENTED_EDGE('',*,*,#1442,.T.);
#1937=ORIENTED_EDGE('',*,*,#1443,.F.);
#1938=ORIENTED_EDGE('',*,*,#1442,.F.);
#1939=ORIENTED_EDGE('',*,*,#1444,.F.);
#1940=ORIENTED_EDGE('',*,*,#1445,.T.);
#1941=ORIENTED_EDGE('',*,*,#1446,.T.);
#1942=ORIENTED_EDGE('',*,*,#1447,.F.);
#1943=ORIENTED_EDGE('',*,*,#1448,.F.);
#1944=ORIENTED_EDGE('',*,*,#1449,.F.);
#1945=ORIENTED_EDGE('',*,*,#1447,.T.);
#1946=ORIENTED_EDGE('',*,*,#1450,.T.);
#1947=ORIENTED_EDGE('',*,*,#1451,.T.);
#1948=ORIENTED_EDGE('',*,*,#1452,.T.);
#1949=ORIENTED_EDGE('',*,*,#1453,.F.);
#1950=ORIENTED_EDGE('',*,*,#1445,.F.);
#1951=ORIENTED_EDGE('',*,*,#1454,.F.);
#1952=ORIENTED_EDGE('',*,*,#1451,.F.);
#1953=ORIENTED_EDGE('',*,*,#1444,.T.);
#1954=ORIENTED_EDGE('',*,*,#1449,.T.);
#1955=ORIENTED_EDGE('',*,*,#1453,.T.);
#1956=ORIENTED_EDGE('',*,*,#1455,.T.);
#1957=ORIENTED_EDGE('',*,*,#1450,.F.);
#1958=ORIENTED_EDGE('',*,*,#1446,.F.);
#1959=ORIENTED_EDGE('',*,*,#1443,.T.);
#1960=ORIENTED_EDGE('',*,*,#1438,.F.);
#1961=ORIENTED_EDGE('',*,*,#1441,.F.);
#1962=ORIENTED_EDGE('',*,*,#1440,.T.);
#1963=ORIENTED_EDGE('',*,*,#1435,.F.);
#1964=ORIENTED_EDGE('',*,*,#1452,.F.);
#1965=ORIENTED_EDGE('',*,*,#1454,.T.);
#1966=ORIENTED_EDGE('',*,*,#1448,.T.);
#1967=ORIENTED_EDGE('',*,*,#1455,.F.);
#1968=ORIENTED_EDGE('',*,*,#1437,.T.);
#1969=ORIENTED_EDGE('',*,*,#1456,.T.);
#1970=ORIENTED_EDGE('',*,*,#1431,.T.);
#1971=ORIENTED_EDGE('',*,*,#1428,.T.);
#1972=ORIENTED_EDGE('',*,*,#1457,.T.);
#1973=ORIENTED_EDGE('',*,*,#1427,.F.);
#1974=ORIENTED_EDGE('',*,*,#1433,.F.);
#1975=ORIENTED_EDGE('',*,*,#1458,.F.);
#1976=ORIENTED_EDGE('',*,*,#1429,.T.);
#1977=ORIENTED_EDGE('',*,*,#1457,.F.);
#1978=ORIENTED_EDGE('',*,*,#1432,.F.);
#1979=ORIENTED_EDGE('',*,*,#1456,.F.);
#1980=ORIENTED_EDGE('',*,*,#1434,.T.);
#1981=ORIENTED_EDGE('',*,*,#1430,.T.);
#1982=ORIENTED_EDGE('',*,*,#1458,.T.);
#1983=ORIENTED_EDGE('',*,*,#1459,.T.);
#1984=ORIENTED_EDGE('',*,*,#1460,.T.);
#1985=ORIENTED_EDGE('',*,*,#1461,.F.);
#1986=ORIENTED_EDGE('',*,*,#1460,.F.);
#1987=ORIENTED_EDGE('',*,*,#1462,.T.);
#1988=ORIENTED_EDGE('',*,*,#1463,.T.);
#1989=ORIENTED_EDGE('',*,*,#1464,.F.);
#1990=ORIENTED_EDGE('',*,*,#1465,.F.);
#1991=ORIENTED_EDGE('',*,*,#1466,.F.);
#1992=ORIENTED_EDGE('',*,*,#1467,.F.);
#1993=ORIENTED_EDGE('',*,*,#1468,.T.);
#1994=ORIENTED_EDGE('',*,*,#1469,.T.);
#1995=ORIENTED_EDGE('',*,*,#1470,.F.);
#1996=ORIENTED_EDGE('',*,*,#1471,.F.);
#1997=ORIENTED_EDGE('',*,*,#1472,.T.);
#1998=ORIENTED_EDGE('',*,*,#1473,.T.);
#1999=ORIENTED_EDGE('',*,*,#1474,.F.);
#2000=ORIENTED_EDGE('',*,*,#1475,.F.);
#2001=ORIENTED_EDGE('',*,*,#1476,.T.);
#2002=ORIENTED_EDGE('',*,*,#1477,.T.);
#2003=ORIENTED_EDGE('',*,*,#1478,.F.);
#2004=ORIENTED_EDGE('',*,*,#1479,.F.);
#2005=ORIENTED_EDGE('',*,*,#1480,.T.);
#2006=ORIENTED_EDGE('',*,*,#1481,.T.);
#2007=ORIENTED_EDGE('',*,*,#1482,.F.);
#2008=ORIENTED_EDGE('',*,*,#1483,.F.);
#2009=ORIENTED_EDGE('',*,*,#1484,.T.);
#2010=ORIENTED_EDGE('',*,*,#1485,.T.);
#2011=ORIENTED_EDGE('',*,*,#1486,.F.);
#2012=ORIENTED_EDGE('',*,*,#1487,.F.);
#2013=ORIENTED_EDGE('',*,*,#1488,.T.);
#2014=ORIENTED_EDGE('',*,*,#1489,.T.);
#2015=ORIENTED_EDGE('',*,*,#1490,.F.);
#2016=ORIENTED_EDGE('',*,*,#1491,.F.);
#2017=ORIENTED_EDGE('',*,*,#1492,.T.);
#2018=ORIENTED_EDGE('',*,*,#1493,.T.);
#2019=ORIENTED_EDGE('',*,*,#1494,.F.);
#2020=ORIENTED_EDGE('',*,*,#1495,.F.);
#2021=ORIENTED_EDGE('',*,*,#1496,.T.);
#2022=ORIENTED_EDGE('',*,*,#1497,.T.);
#2023=ORIENTED_EDGE('',*,*,#1498,.F.);
#2024=ORIENTED_EDGE('',*,*,#1499,.T.);
#2025=ORIENTED_EDGE('',*,*,#1500,.T.);
#2026=ORIENTED_EDGE('',*,*,#1501,.T.);
#2027=ORIENTED_EDGE('',*,*,#1502,.F.);
#2028=ORIENTED_EDGE('',*,*,#1503,.F.);
#2029=ORIENTED_EDGE('',*,*,#1504,.F.);
#2030=ORIENTED_EDGE('',*,*,#1505,.T.);
#2031=ORIENTED_EDGE('',*,*,#1506,.F.);
#2032=ORIENTED_EDGE('',*,*,#1507,.F.);
#2033=ORIENTED_EDGE('',*,*,#1508,.T.);
#2034=ORIENTED_EDGE('',*,*,#1504,.T.);
#2035=ORIENTED_EDGE('',*,*,#1509,.T.);
#2036=ORIENTED_EDGE('',*,*,#1510,.T.);
#2037=ORIENTED_EDGE('',*,*,#1511,.F.);
#2038=ORIENTED_EDGE('',*,*,#1507,.T.);
#2039=ORIENTED_EDGE('',*,*,#1500,.F.);
#2040=ORIENTED_EDGE('',*,*,#1512,.T.);
#2041=ORIENTED_EDGE('',*,*,#1463,.F.);
#2042=ORIENTED_EDGE('',*,*,#1513,.T.);
#2043=ORIENTED_EDGE('',*,*,#1469,.F.);
#2044=ORIENTED_EDGE('',*,*,#1514,.T.);
#2045=ORIENTED_EDGE('',*,*,#1473,.F.);
#2046=ORIENTED_EDGE('',*,*,#1515,.T.);
#2047=ORIENTED_EDGE('',*,*,#1477,.F.);
#2048=ORIENTED_EDGE('',*,*,#1516,.T.);
#2049=ORIENTED_EDGE('',*,*,#1481,.F.);
#2050=ORIENTED_EDGE('',*,*,#1517,.T.);
#2051=ORIENTED_EDGE('',*,*,#1485,.F.);
#2052=ORIENTED_EDGE('',*,*,#1518,.T.);
#2053=ORIENTED_EDGE('',*,*,#1489,.F.);
#2054=ORIENTED_EDGE('',*,*,#1519,.T.);
#2055=ORIENTED_EDGE('',*,*,#1493,.F.);
#2056=ORIENTED_EDGE('',*,*,#1520,.T.);
#2057=ORIENTED_EDGE('',*,*,#1497,.F.);
#2058=ORIENTED_EDGE('',*,*,#1521,.T.);
#2059=ORIENTED_EDGE('',*,*,#1505,.F.);
#2060=ORIENTED_EDGE('',*,*,#1508,.F.);
#2061=ORIENTED_EDGE('',*,*,#1511,.T.);
#2062=ORIENTED_EDGE('',*,*,#1522,.T.);
#2063=ORIENTED_EDGE('',*,*,#1523,.T.);
#2064=ORIENTED_EDGE('',*,*,#1461,.T.);
#2065=ORIENTED_EDGE('',*,*,#1503,.T.);
#2066=ORIENTED_EDGE('',*,*,#1524,.T.);
#2067=ORIENTED_EDGE('',*,*,#1495,.T.);
#2068=ORIENTED_EDGE('',*,*,#1525,.T.);
#2069=ORIENTED_EDGE('',*,*,#1491,.T.);
#2070=ORIENTED_EDGE('',*,*,#1526,.T.);
#2071=ORIENTED_EDGE('',*,*,#1487,.T.);
#2072=ORIENTED_EDGE('',*,*,#1527,.T.);
#2073=ORIENTED_EDGE('',*,*,#1483,.T.);
#2074=ORIENTED_EDGE('',*,*,#1528,.T.);
#2075=ORIENTED_EDGE('',*,*,#1479,.T.);
#2076=ORIENTED_EDGE('',*,*,#1529,.T.);
#2077=ORIENTED_EDGE('',*,*,#1475,.T.);
#2078=ORIENTED_EDGE('',*,*,#1530,.T.);
#2079=ORIENTED_EDGE('',*,*,#1471,.T.);
#2080=ORIENTED_EDGE('',*,*,#1531,.T.);
#2081=ORIENTED_EDGE('',*,*,#1467,.T.);
#2082=ORIENTED_EDGE('',*,*,#1532,.T.);
#2083=ORIENTED_EDGE('',*,*,#1465,.T.);
#2084=ORIENTED_EDGE('',*,*,#1533,.T.);
#2085=ORIENTED_EDGE('',*,*,#1498,.T.);
#2086=ORIENTED_EDGE('',*,*,#1534,.T.);
#2087=ORIENTED_EDGE('',*,*,#1535,.T.);
#2088=ORIENTED_EDGE('',*,*,#1509,.F.);
#2089=ORIENTED_EDGE('',*,*,#1506,.T.);
#2090=ORIENTED_EDGE('',*,*,#1459,.F.);
#2091=ORIENTED_EDGE('',*,*,#1535,.F.);
#2092=ORIENTED_EDGE('',*,*,#1536,.T.);
#2093=ORIENTED_EDGE('',*,*,#1522,.F.);
#2094=ORIENTED_EDGE('',*,*,#1510,.F.);
#2095=ORIENTED_EDGE('',*,*,#1523,.F.);
#2096=ORIENTED_EDGE('',*,*,#1536,.F.);
#2097=ORIENTED_EDGE('',*,*,#1534,.F.);
#2098=ORIENTED_EDGE('',*,*,#1501,.F.);
#2099=ORIENTED_EDGE('',*,*,#1499,.F.);
#2100=ORIENTED_EDGE('',*,*,#1537,.T.);
#2101=ORIENTED_EDGE('',*,*,#1538,.T.);
#2102=ORIENTED_EDGE('',*,*,#1539,.F.);
#2103=ORIENTED_EDGE('',*,*,#1512,.F.);
#2104=ORIENTED_EDGE('',*,*,#1538,.F.);
#2105=ORIENTED_EDGE('',*,*,#1540,.F.);
#2106=ORIENTED_EDGE('',*,*,#1464,.T.);
#2107=ORIENTED_EDGE('',*,*,#1539,.T.);
#2108=ORIENTED_EDGE('',*,*,#1533,.F.);
#2109=ORIENTED_EDGE('',*,*,#1540,.T.);
#2110=ORIENTED_EDGE('',*,*,#1537,.F.);
#2111=ORIENTED_EDGE('',*,*,#1496,.F.);
#2112=ORIENTED_EDGE('',*,*,#1541,.T.);
#2113=ORIENTED_EDGE('',*,*,#1542,.T.);
#2114=ORIENTED_EDGE('',*,*,#1543,.F.);
#2115=ORIENTED_EDGE('',*,*,#1521,.F.);
#2116=ORIENTED_EDGE('',*,*,#1542,.F.);
#2117=ORIENTED_EDGE('',*,*,#1544,.F.);
#2118=ORIENTED_EDGE('',*,*,#1502,.T.);
#2119=ORIENTED_EDGE('',*,*,#1543,.T.);
#2120=ORIENTED_EDGE('',*,*,#1524,.F.);
#2121=ORIENTED_EDGE('',*,*,#1544,.T.);
#2122=ORIENTED_EDGE('',*,*,#1541,.F.);
#2123=ORIENTED_EDGE('',*,*,#1492,.F.);
#2124=ORIENTED_EDGE('',*,*,#1545,.T.);
#2125=ORIENTED_EDGE('',*,*,#1546,.T.);
#2126=ORIENTED_EDGE('',*,*,#1547,.F.);
#2127=ORIENTED_EDGE('',*,*,#1520,.F.);
#2128=ORIENTED_EDGE('',*,*,#1546,.F.);
#2129=ORIENTED_EDGE('',*,*,#1548,.F.);
#2130=ORIENTED_EDGE('',*,*,#1494,.T.);
#2131=ORIENTED_EDGE('',*,*,#1547,.T.);
#2132=ORIENTED_EDGE('',*,*,#1525,.F.);
#2133=ORIENTED_EDGE('',*,*,#1548,.T.);
#2134=ORIENTED_EDGE('',*,*,#1545,.F.);
#2135=ORIENTED_EDGE('',*,*,#1488,.F.);
#2136=ORIENTED_EDGE('',*,*,#1549,.T.);
#2137=ORIENTED_EDGE('',*,*,#1550,.T.);
#2138=ORIENTED_EDGE('',*,*,#1551,.F.);
#2139=ORIENTED_EDGE('',*,*,#1519,.F.);
#2140=ORIENTED_EDGE('',*,*,#1550,.F.);
#2141=ORIENTED_EDGE('',*,*,#1552,.F.);
#2142=ORIENTED_EDGE('',*,*,#1490,.T.);
#2143=ORIENTED_EDGE('',*,*,#1551,.T.);
#2144=ORIENTED_EDGE('',*,*,#1526,.F.);
#2145=ORIENTED_EDGE('',*,*,#1552,.T.);
#2146=ORIENTED_EDGE('',*,*,#1549,.F.);
#2147=ORIENTED_EDGE('',*,*,#1484,.F.);
#2148=ORIENTED_EDGE('',*,*,#1553,.T.);
#2149=ORIENTED_EDGE('',*,*,#1554,.T.);
#2150=ORIENTED_EDGE('',*,*,#1555,.F.);
#2151=ORIENTED_EDGE('',*,*,#1518,.F.);
#2152=ORIENTED_EDGE('',*,*,#1554,.F.);
#2153=ORIENTED_EDGE('',*,*,#1556,.F.);
#2154=ORIENTED_EDGE('',*,*,#1486,.T.);
#2155=ORIENTED_EDGE('',*,*,#1555,.T.);
#2156=ORIENTED_EDGE('',*,*,#1527,.F.);
#2157=ORIENTED_EDGE('',*,*,#1556,.T.);
#2158=ORIENTED_EDGE('',*,*,#1553,.F.);
#2159=ORIENTED_EDGE('',*,*,#1480,.F.);
#2160=ORIENTED_EDGE('',*,*,#1557,.T.);
#2161=ORIENTED_EDGE('',*,*,#1558,.T.);
#2162=ORIENTED_EDGE('',*,*,#1559,.F.);
#2163=ORIENTED_EDGE('',*,*,#1517,.F.);
#2164=ORIENTED_EDGE('',*,*,#1558,.F.);
#2165=ORIENTED_EDGE('',*,*,#1560,.F.);
#2166=ORIENTED_EDGE('',*,*,#1482,.T.);
#2167=ORIENTED_EDGE('',*,*,#1559,.T.);
#2168=ORIENTED_EDGE('',*,*,#1528,.F.);
#2169=ORIENTED_EDGE('',*,*,#1560,.T.);
#2170=ORIENTED_EDGE('',*,*,#1557,.F.);
#2171=ORIENTED_EDGE('',*,*,#1476,.F.);
#2172=ORIENTED_EDGE('',*,*,#1561,.T.);
#2173=ORIENTED_EDGE('',*,*,#1562,.T.);
#2174=ORIENTED_EDGE('',*,*,#1563,.F.);
#2175=ORIENTED_EDGE('',*,*,#1516,.F.);
#2176=ORIENTED_EDGE('',*,*,#1562,.F.);
#2177=ORIENTED_EDGE('',*,*,#1564,.F.);
#2178=ORIENTED_EDGE('',*,*,#1478,.T.);
#2179=ORIENTED_EDGE('',*,*,#1563,.T.);
#2180=ORIENTED_EDGE('',*,*,#1529,.F.);
#2181=ORIENTED_EDGE('',*,*,#1564,.T.);
#2182=ORIENTED_EDGE('',*,*,#1561,.F.);
#2183=ORIENTED_EDGE('',*,*,#1472,.F.);
#2184=ORIENTED_EDGE('',*,*,#1565,.T.);
#2185=ORIENTED_EDGE('',*,*,#1566,.T.);
#2186=ORIENTED_EDGE('',*,*,#1567,.F.);
#2187=ORIENTED_EDGE('',*,*,#1515,.F.);
#2188=ORIENTED_EDGE('',*,*,#1566,.F.);
#2189=ORIENTED_EDGE('',*,*,#1568,.F.);
#2190=ORIENTED_EDGE('',*,*,#1474,.T.);
#2191=ORIENTED_EDGE('',*,*,#1567,.T.);
#2192=ORIENTED_EDGE('',*,*,#1530,.F.);
#2193=ORIENTED_EDGE('',*,*,#1568,.T.);
#2194=ORIENTED_EDGE('',*,*,#1565,.F.);
#2195=ORIENTED_EDGE('',*,*,#1468,.F.);
#2196=ORIENTED_EDGE('',*,*,#1569,.T.);
#2197=ORIENTED_EDGE('',*,*,#1570,.T.);
#2198=ORIENTED_EDGE('',*,*,#1571,.F.);
#2199=ORIENTED_EDGE('',*,*,#1514,.F.);
#2200=ORIENTED_EDGE('',*,*,#1570,.F.);
#2201=ORIENTED_EDGE('',*,*,#1572,.F.);
#2202=ORIENTED_EDGE('',*,*,#1470,.T.);
#2203=ORIENTED_EDGE('',*,*,#1571,.T.);
#2204=ORIENTED_EDGE('',*,*,#1531,.F.);
#2205=ORIENTED_EDGE('',*,*,#1572,.T.);
#2206=ORIENTED_EDGE('',*,*,#1569,.F.);
#2207=ORIENTED_EDGE('',*,*,#1462,.F.);
#2208=ORIENTED_EDGE('',*,*,#1573,.T.);
#2209=ORIENTED_EDGE('',*,*,#1574,.T.);
#2210=ORIENTED_EDGE('',*,*,#1575,.F.);
#2211=ORIENTED_EDGE('',*,*,#1513,.F.);
#2212=ORIENTED_EDGE('',*,*,#1574,.F.);
#2213=ORIENTED_EDGE('',*,*,#1576,.F.);
#2214=ORIENTED_EDGE('',*,*,#1466,.T.);
#2215=ORIENTED_EDGE('',*,*,#1575,.T.);
#2216=ORIENTED_EDGE('',*,*,#1532,.F.);
#2217=ORIENTED_EDGE('',*,*,#1576,.T.);
#2218=ORIENTED_EDGE('',*,*,#1573,.F.);
#2219=ORIENTED_EDGE('',*,*,#1577,.T.);
#2220=ORIENTED_EDGE('',*,*,#1578,.T.);
#2221=ORIENTED_EDGE('',*,*,#1579,.F.);
#2222=ORIENTED_EDGE('',*,*,#1578,.F.);
#2223=ORIENTED_EDGE('',*,*,#1579,.T.);
#2224=ORIENTED_EDGE('',*,*,#1577,.F.);
#2225=ORIENTED_EDGE('',*,*,#1580,.T.);
#2226=ORIENTED_EDGE('',*,*,#1581,.T.);
#2227=ORIENTED_EDGE('',*,*,#1582,.F.);
#2228=ORIENTED_EDGE('',*,*,#1581,.F.);
#2229=ORIENTED_EDGE('',*,*,#1582,.T.);
#2230=ORIENTED_EDGE('',*,*,#1580,.F.);
#2231=CYLINDRICAL_SURFACE('',#2480,1.25);
#2232=CYLINDRICAL_SURFACE('',#2483,1.25);
#2233=CYLINDRICAL_SURFACE('',#2486,1.5);
#2234=CYLINDRICAL_SURFACE('',#2489,1.5);
#2235=CYLINDRICAL_SURFACE('',#2492,49.);
#2236=CYLINDRICAL_SURFACE('',#2495,44.);
#2237=CYLINDRICAL_SURFACE('',#2498,50.);
#2238=CYLINDRICAL_SURFACE('',#2501,44.);
#2239=CYLINDRICAL_SURFACE('',#2506,4.99999999999999);
#2240=CYLINDRICAL_SURFACE('',#2511,106.);
#2241=CYLINDRICAL_SURFACE('',#2517,4.99999999999999);
#2242=CYLINDRICAL_SURFACE('',#2520,100.);
#2243=CYLINDRICAL_SURFACE('',#2523,106.);
#2244=CYLINDRICAL_SURFACE('',#2529,101.);
#2245=CYLINDRICAL_SURFACE('',#2536,0.5);
#2246=CYLINDRICAL_SURFACE('',#2540,1.25);
#2247=CYLINDRICAL_SURFACE('',#2543,1.25);
#2248=CYLINDRICAL_SURFACE('',#2546,7.5);
#2249=CYLINDRICAL_SURFACE('',#2549,0.5);
#2250=CYLINDRICAL_SURFACE('',#2552,0.5);
#2251=CYLINDRICAL_SURFACE('',#2555,7.5);
#2252=CYLINDRICAL_SURFACE('',#2565,4.);
#2253=CYLINDRICAL_SURFACE('',#2580,4.);
#2254=CYLINDRICAL_SURFACE('',#2593,3.);
#2255=CYLINDRICAL_SURFACE('',#2596,1.5);
#2256=CYLINDRICAL_SURFACE('',#2599,2.5);
#2257=CYLINDRICAL_SURFACE('',#2614,1.25);
#2258=CYLINDRICAL_SURFACE('',#2636,20.5);
#2259=CYLINDRICAL_SURFACE('',#2637,0.5);
#2260=CYLINDRICAL_SURFACE('',#2679,1.25);
#2261=CYLINDRICAL_SURFACE('',#2685,1.5);
#2262=ADVANCED_FACE('',(#194),#2231,.F.);
#2263=ADVANCED_FACE('',(#195),#2232,.F.);
#2264=ADVANCED_FACE('',(#196),#2233,.F.);
#2265=ADVANCED_FACE('',(#197),#2234,.F.);
#2266=ADVANCED_FACE('',(#198),#2235,.F.);
#2267=ADVANCED_FACE('',(#199),#2236,.F.);
#2268=ADVANCED_FACE('',(#200),#2237,.T.);
#2269=ADVANCED_FACE('',(#201),#2238,.F.);
#2270=ADVANCED_FACE('',(#202),#86,.F.);
#2271=ADVANCED_FACE('',(#203),#87,.F.);
#2272=ADVANCED_FACE('',(#204),#2239,.T.);
#2273=ADVANCED_FACE('',(#205),#88,.T.);
#2274=ADVANCED_FACE('',(#206),#89,.F.);
#2275=ADVANCED_FACE('',(#207),#2240,.T.);
#2276=ADVANCED_FACE('',(#208),#90,.F.);
#2277=ADVANCED_FACE('',(#209),#91,.F.);
#2278=ADVANCED_FACE('',(#210),#92,.F.);
#2279=ADVANCED_FACE('',(#211),#2241,.T.);
#2280=ADVANCED_FACE('',(#212),#2242,.F.);
#2281=ADVANCED_FACE('',(#213),#2243,.T.);
#2282=ADVANCED_FACE('',(#214),#93,.F.);
#2283=ADVANCED_FACE('',(#215,#71),#94,.T.);
#2284=ADVANCED_FACE('',(#216,#72),#95,.F.);
#2285=ADVANCED_FACE('',(#217),#2244,.T.);
#2286=ADVANCED_FACE('',(#218,#73,#74),#96,.F.);
#2287=ADVANCED_FACE('',(#219,#75,#76),#97,.T.);
#2288=ADVANCED_FACE('',(#220),#2245,.T.);
#2289=ADVANCED_FACE('',(#221),#98,.T.);
#2290=ADVANCED_FACE('',(#222),#99,.F.);
#2291=ADVANCED_FACE('',(#223),#2246,.F.);
#2292=ADVANCED_FACE('',(#224),#2247,.F.);
#2293=ADVANCED_FACE('',(#225),#2248,.T.);
#2294=ADVANCED_FACE('',(#226),#2249,.T.);
#2295=ADVANCED_FACE('',(#227),#2250,.T.);
#2296=ADVANCED_FACE('',(#228),#2251,.T.);
#2297=ADVANCED_FACE('',(#229),#100,.F.);
#2298=ADVANCED_FACE('',(#230),#101,.F.);
#2299=ADVANCED_FACE('',(#231),#102,.F.);
#2300=ADVANCED_FACE('',(#232),#103,.F.);
#2301=ADVANCED_FACE('',(#233),#104,.F.);
#2302=ADVANCED_FACE('',(#234),#105,.F.);
#2303=ADVANCED_FACE('',(#235),#106,.F.);
#2304=ADVANCED_FACE('',(#236),#2252,.F.);
#2305=ADVANCED_FACE('',(#237),#107,.F.);
#2306=ADVANCED_FACE('',(#238),#108,.F.);
#2307=ADVANCED_FACE('',(#239),#109,.F.);
#2308=ADVANCED_FACE('',(#240),#110,.F.);
#2309=ADVANCED_FACE('',(#241),#111,.F.);
#2310=ADVANCED_FACE('',(#242),#112,.F.);
#2311=ADVANCED_FACE('',(#243),#113,.F.);
#2312=ADVANCED_FACE('',(#244),#114,.F.);
#2313=ADVANCED_FACE('',(#245),#115,.F.);
#2314=ADVANCED_FACE('',(#246),#116,.T.);
#2315=ADVANCED_FACE('',(#247),#117,.T.);
#2316=ADVANCED_FACE('',(#248),#2253,.F.);
#2317=ADVANCED_FACE('',(#249),#118,.T.);
#2318=ADVANCED_FACE('',(#250),#119,.F.);
#2319=ADVANCED_FACE('',(#251),#120,.T.);
#2320=ADVANCED_FACE('',(#252),#121,.T.);
#2321=ADVANCED_FACE('',(#253,#77),#122,.T.);
#2322=ADVANCED_FACE('',(#254,#78),#123,.F.);
#2323=ADVANCED_FACE('',(#255),#124,.T.);
#2324=ADVANCED_FACE('',(#256),#125,.F.);
#2325=ADVANCED_FACE('',(#257),#45,.T.);
#2326=ADVANCED_FACE('',(#258),#35,.T.);
#2327=ADVANCED_FACE('',(#259),#2254,.T.);
#2328=ADVANCED_FACE('',(#260),#2255,.F.);
#2329=ADVANCED_FACE('',(#261,#79),#2256,.T.);
#2330=ADVANCED_FACE('',(#262),#126,.F.);
#2331=ADVANCED_FACE('',(#263),#127,.T.);
#2332=ADVANCED_FACE('',(#264),#128,.F.);
#2333=ADVANCED_FACE('',(#265),#129,.T.);
#2334=ADVANCED_FACE('',(#266,#80),#130,.T.);
#2335=ADVANCED_FACE('',(#267,#81),#131,.F.);
#2336=ADVANCED_FACE('',(#268,#82),#132,.F.);
#2337=ADVANCED_FACE('',(#269,#83),#133,.T.);
#2338=ADVANCED_FACE('',(#270),#134,.F.);
#2339=ADVANCED_FACE('',(#271),#46,.T.);
#2340=ADVANCED_FACE('',(#272),#36,.T.);
#2341=ADVANCED_FACE('',(#273),#2257,.F.);
#2342=ADVANCED_FACE('',(#274),#135,.T.);
#2343=ADVANCED_FACE('',(#275),#136,.T.);
#2344=ADVANCED_FACE('',(#276),#137,.T.);
#2345=ADVANCED_FACE('',(#277),#138,.T.);
#2346=ADVANCED_FACE('',(#278),#139,.T.);
#2347=ADVANCED_FACE('',(#279),#140,.T.);
#2348=ADVANCED_FACE('',(#280),#141,.T.);
#2349=ADVANCED_FACE('',(#281),#142,.T.);
#2350=ADVANCED_FACE('',(#282),#143,.T.);
#2351=ADVANCED_FACE('',(#283),#144,.T.);
#2352=ADVANCED_FACE('',(#284),#145,.T.);
#2353=ADVANCED_FACE('',(#285),#146,.T.);
#2354=ADVANCED_FACE('',(#286),#147,.F.);
#2355=ADVANCED_FACE('',(#287,#84),#148,.F.);
#2356=ADVANCED_FACE('',(#288,#85),#149,.T.);
#2357=ADVANCED_FACE('',(#289),#2258,.T.);
#2358=ADVANCED_FACE('',(#290),#2259,.T.);
#2359=ADVANCED_FACE('',(#291),#150,.T.);
#2360=ADVANCED_FACE('',(#292),#151,.F.);
#2361=ADVANCED_FACE('',(#293),#152,.F.);
#2362=ADVANCED_FACE('',(#294),#153,.T.);
#2363=ADVANCED_FACE('',(#295),#154,.T.);
#2364=ADVANCED_FACE('',(#296),#155,.F.);
#2365=ADVANCED_FACE('',(#297),#156,.F.);
#2366=ADVANCED_FACE('',(#298),#157,.T.);
#2367=ADVANCED_FACE('',(#299),#158,.T.);
#2368=ADVANCED_FACE('',(#300),#159,.F.);
#2369=ADVANCED_FACE('',(#301),#160,.F.);
#2370=ADVANCED_FACE('',(#302),#161,.T.);
#2371=ADVANCED_FACE('',(#303),#162,.T.);
#2372=ADVANCED_FACE('',(#304),#163,.F.);
#2373=ADVANCED_FACE('',(#305),#164,.F.);
#2374=ADVANCED_FACE('',(#306),#165,.T.);
#2375=ADVANCED_FACE('',(#307),#166,.T.);
#2376=ADVANCED_FACE('',(#308),#167,.F.);
#2377=ADVANCED_FACE('',(#309),#168,.F.);
#2378=ADVANCED_FACE('',(#310),#169,.T.);
#2379=ADVANCED_FACE('',(#311),#170,.T.);
#2380=ADVANCED_FACE('',(#312),#171,.F.);
#2381=ADVANCED_FACE('',(#313),#172,.F.);
#2382=ADVANCED_FACE('',(#314),#173,.T.);
#2383=ADVANCED_FACE('',(#315),#174,.T.);
#2384=ADVANCED_FACE('',(#316),#175,.F.);
#2385=ADVANCED_FACE('',(#317),#176,.F.);
#2386=ADVANCED_FACE('',(#318),#177,.T.);
#2387=ADVANCED_FACE('',(#319),#178,.T.);
#2388=ADVANCED_FACE('',(#320),#179,.F.);
#2389=ADVANCED_FACE('',(#321),#180,.F.);
#2390=ADVANCED_FACE('',(#322),#181,.T.);
#2391=ADVANCED_FACE('',(#323),#182,.T.);
#2392=ADVANCED_FACE('',(#324),#183,.F.);
#2393=ADVANCED_FACE('',(#325),#184,.F.);
#2394=ADVANCED_FACE('',(#326),#185,.T.);
#2395=ADVANCED_FACE('',(#327),#186,.T.);
#2396=ADVANCED_FACE('',(#328),#187,.F.);
#2397=ADVANCED_FACE('',(#329),#188,.F.);
#2398=ADVANCED_FACE('',(#330),#189,.T.);
#2399=ADVANCED_FACE('',(#331),#2260,.T.);
#2400=ADVANCED_FACE('',(#332),#190,.T.);
#2401=ADVANCED_FACE('',(#333),#191,.F.);
#2402=ADVANCED_FACE('',(#334),#2261,.T.);
#2403=ADVANCED_FACE('',(#335),#192,.T.);
#2404=ADVANCED_FACE('',(#336),#193,.F.);
#2405=CLOSED_SHELL('',(#2262,#2263,#2264,#2265,#2266,#2267,#2268,#2269,
#2270,#2271,#2272,#2273,#2274,#2275,#2276,#2277,#2278,#2279,#2280,#2281,
#2282,#2283,#2284,#2285,#2286,#2287,#2288,#2289,#2290));
#2406=CLOSED_SHELL('',(#2291,#2292,#2293,#2294,#2295,#2296,#2297,#2298,
#2299,#2300,#2301,#2302,#2303,#2304,#2305,#2306,#2307,#2308,#2309,#2310,
#2311,#2312,#2313,#2314,#2315,#2316,#2317,#2318,#2319,#2320,#2321,#2322,
#2323,#2324));
#2407=CLOSED_SHELL('',(#2325,#2326,#2327,#2328,#2329,#2330,#2331,#2332,
#2333,#2334,#2335,#2336,#2337,#2338,#2339,#2340));
#2408=CLOSED_SHELL('',(#2341,#2342,#2343,#2344,#2345,#2346,#2347,#2348,
#2349,#2350,#2351,#2352,#2353,#2354,#2355,#2356,#2357,#2358,#2359,#2360,
#2361,#2362,#2363,#2364,#2365,#2366,#2367,#2368,#2369,#2370,#2371,#2372,
#2373,#2374,#2375,#2376,#2377,#2378,#2379,#2380,#2381,#2382,#2383,#2384,
#2385,#2386,#2387,#2388,#2389,#2390,#2391,#2392,#2393,#2394,#2395,#2396,
#2397,#2398));
#2409=CLOSED_SHELL('',(#2399,#2400,#2401));
#2410=CLOSED_SHELL('',(#2402,#2403,#2404));
#2411=DERIVED_UNIT_ELEMENT(#2423,1.);
#2412=DERIVED_UNIT_ELEMENT(#9563,-3.);
#2413=DERIVED_UNIT_ELEMENT(#2423,1.);
#2414=DERIVED_UNIT_ELEMENT(#9563,-3.);
#2415=DERIVED_UNIT_ELEMENT(#2423,1.);
#2416=DERIVED_UNIT_ELEMENT(#9563,-3.);
#2417=DERIVED_UNIT_ELEMENT(#2423,1.);
#2418=DERIVED_UNIT_ELEMENT(#9563,-3.);
#2419=DERIVED_UNIT_ELEMENT(#2423,1.);
#2420=DERIVED_UNIT_ELEMENT(#9563,-3.);
#2421=DERIVED_UNIT_ELEMENT(#2423,1.);
#2422=DERIVED_UNIT_ELEMENT(#9563,-3.);
#2423=(
MASS_UNIT()
NAMED_UNIT(*)
SI_UNIT(.KILO.,.GRAM.)
);
#2424=DERIVED_UNIT((#2411,#2412));
#2425=DERIVED_UNIT((#2413,#2414));
#2426=DERIVED_UNIT((#2415,#2416));
#2427=DERIVED_UNIT((#2417,#2418));
#2428=DERIVED_UNIT((#2419,#2420));
#2429=DERIVED_UNIT((#2421,#2422));
#2430=MEASURE_REPRESENTATION_ITEM('density measure',
POSITIVE_RATIO_MEASURE(7850.),#2424);
#2431=MEASURE_REPRESENTATION_ITEM('density measure',
POSITIVE_RATIO_MEASURE(7850.),#2425);
#2432=MEASURE_REPRESENTATION_ITEM('density measure',
POSITIVE_RATIO_MEASURE(7850.),#2426);
#2433=MEASURE_REPRESENTATION_ITEM('density measure',
POSITIVE_RATIO_MEASURE(7850.),#2427);
#2434=MEASURE_REPRESENTATION_ITEM('density measure',
POSITIVE_RATIO_MEASURE(7850.),#2428);
#2435=MEASURE_REPRESENTATION_ITEM('density measure',
POSITIVE_RATIO_MEASURE(7850.),#2429);
#2436=PROPERTY_DEFINITION_REPRESENTATION(#2466,#2448);
#2437=PROPERTY_DEFINITION_REPRESENTATION(#2467,#2449);
#2438=PROPERTY_DEFINITION_REPRESENTATION(#2468,#2450);
#2439=PROPERTY_DEFINITION_REPRESENTATION(#2469,#2451);
#2440=PROPERTY_DEFINITION_REPRESENTATION(#2470,#2452);
#2441=PROPERTY_DEFINITION_REPRESENTATION(#2471,#2453);
#2442=PROPERTY_DEFINITION_REPRESENTATION(#2472,#2454);
#2443=PROPERTY_DEFINITION_REPRESENTATION(#2473,#2455);
#2444=PROPERTY_DEFINITION_REPRESENTATION(#2474,#2456);
#2445=PROPERTY_DEFINITION_REPRESENTATION(#2475,#2457);
#2446=PROPERTY_DEFINITION_REPRESENTATION(#2476,#2458);
#2447=PROPERTY_DEFINITION_REPRESENTATION(#2477,#2459);
#2448=REPRESENTATION('material name',(#2460),#9555);
#2449=REPRESENTATION('density',(#2430),#9555);
#2450=REPRESENTATION('material name',(#2461),#9556);
#2451=REPRESENTATION('density',(#2431),#9556);
#2452=REPRESENTATION('material name',(#2462),#9557);
#2453=REPRESENTATION('density',(#2432),#9557);
#2454=REPRESENTATION('material name',(#2463),#9558);
#2455=REPRESENTATION('density',(#2433),#9558);
#2456=REPRESENTATION('material name',(#2464),#9559);
#2457=REPRESENTATION('density',(#2434),#9559);
#2458=REPRESENTATION('material name',(#2465),#9560);
#2459=REPRESENTATION('density',(#2435),#9560);
#2460=DESCRIPTIVE_REPRESENTATION_ITEM('Steel','Steel');
#2461=DESCRIPTIVE_REPRESENTATION_ITEM('Steel','Steel');
#2462=DESCRIPTIVE_REPRESENTATION_ITEM('Steel','Steel');
#2463=DESCRIPTIVE_REPRESENTATION_ITEM('Steel','Steel');
#2464=DESCRIPTIVE_REPRESENTATION_ITEM('Steel','Steel');
#2465=DESCRIPTIVE_REPRESENTATION_ITEM('Steel','Steel');
#2466=PROPERTY_DEFINITION('material property','material name',#9595);
#2467=PROPERTY_DEFINITION('material property','density of part',#9595);
#2468=PROPERTY_DEFINITION('material property','material name',#9596);
#2469=PROPERTY_DEFINITION('material property','density of part',#9596);
#2470=PROPERTY_DEFINITION('material property','material name',#9597);
#2471=PROPERTY_DEFINITION('material property','density of part',#9597);
#2472=PROPERTY_DEFINITION('material property','material name',#9598);
#2473=PROPERTY_DEFINITION('material property','density of part',#9598);
#2474=PROPERTY_DEFINITION('material property','material name',#9599);
#2475=PROPERTY_DEFINITION('material property','density of part',#9599);
#2476=PROPERTY_DEFINITION('material property','material name',#9600);
#2477=PROPERTY_DEFINITION('material property','density of part',#9600);
#2478=AXIS2_PLACEMENT_3D('',#3382,#2696,#2697);
#2479=AXIS2_PLACEMENT_3D('',#3383,#2698,#2699);
#2480=AXIS2_PLACEMENT_3D('',#3384,#2700,#2701);
#2481=AXIS2_PLACEMENT_3D('',#3386,#2702,#2703);
#2482=AXIS2_PLACEMENT_3D('',#3389,#2705,#2706);
#2483=AXIS2_PLACEMENT_3D('',#3390,#2707,#2708);
#2484=AXIS2_PLACEMENT_3D('',#3392,#2709,#2710);
#2485=AXIS2_PLACEMENT_3D('',#3395,#2712,#2713);
#2486=AXIS2_PLACEMENT_3D('',#3396,#2714,#2715);
#2487=AXIS2_PLACEMENT_3D('',#3398,#2716,#2717);
#2488=AXIS2_PLACEMENT_3D('',#3401,#2719,#2720);
#2489=AXIS2_PLACEMENT_3D('',#3402,#2721,#2722);
#2490=AXIS2_PLACEMENT_3D('',#3404,#2723,#2724);
#2491=AXIS2_PLACEMENT_3D('',#3407,#2726,#2727);
#2492=AXIS2_PLACEMENT_3D('',#3408,#2728,#2729);
#2493=AXIS2_PLACEMENT_3D('',#3411,#2730,#2731);
#2494=AXIS2_PLACEMENT_3D('',#3415,#2733,#2734);
#2495=AXIS2_PLACEMENT_3D('',#3417,#2736,#2737);
#2496=AXIS2_PLACEMENT_3D('',#3420,#2738,#2739);
#2497=AXIS2_PLACEMENT_3D('',#3424,#2741,#2742);
#2498=AXIS2_PLACEMENT_3D('',#3426,#2744,#2745);
#2499=AXIS2_PLACEMENT_3D('',#3429,#2746,#2747);
#2500=AXIS2_PLACEMENT_3D('',#3433,#2749,#2750);
#2501=AXIS2_PLACEMENT_3D('',#3435,#2752,#2753);
#2502=AXIS2_PLACEMENT_3D('',#3438,#2754,#2755);
#2503=AXIS2_PLACEMENT_3D('',#3442,#2757,#2758);
#2504=AXIS2_PLACEMENT_3D('',#3444,#2760,#2761);
#2505=AXIS2_PLACEMENT_3D('',#3453,#2766,#2767);
#2506=AXIS2_PLACEMENT_3D('',#3459,#2771,#2772);
#2507=AXIS2_PLACEMENT_3D('',#3461,#2773,#2774);
#2508=AXIS2_PLACEMENT_3D('',#3463,#2775,#2776);
#2509=AXIS2_PLACEMENT_3D('',#3465,#2778,#2779);
#2510=AXIS2_PLACEMENT_3D('',#3479,#2787,#2788);
#2511=AXIS2_PLACEMENT_3D('',#3484,#2793,#2794);
#2512=AXIS2_PLACEMENT_3D('',#3486,#2795,#2796);
#2513=AXIS2_PLACEMENT_3D('',#3488,#2797,#2798);
#2514=AXIS2_PLACEMENT_3D('',#3490,#2800,#2801);
#2515=AXIS2_PLACEMENT_3D('',#3493,#2804,#2805);
#2516=AXIS2_PLACEMENT_3D('',#3502,#2810,#2811);
#2517=AXIS2_PLACEMENT_3D('',#3508,#2815,#2816);
#2518=AXIS2_PLACEMENT_3D('',#3509,#2817,#2818);
#2519=AXIS2_PLACEMENT_3D('',#3510,#2819,#2820);
#2520=AXIS2_PLACEMENT_3D('',#3511,#2821,#2822);
#2521=AXIS2_PLACEMENT_3D('',#3512,#2823,#2824);
#2522=AXIS2_PLACEMENT_3D('',#3513,#2825,#2826);
#2523=AXIS2_PLACEMENT_3D('',#3514,#2827,#2828);
#2524=AXIS2_PLACEMENT_3D('',#3516,#2829,#2830);
#2525=AXIS2_PLACEMENT_3D('',#3519,#2832,#2833);
#2526=AXIS2_PLACEMENT_3D('',#3520,#2834,#2835);
#2527=AXIS2_PLACEMENT_3D('',#3523,#2838,#2839);
#2528=AXIS2_PLACEMENT_3D('',#3524,#2840,#2841);
#2529=AXIS2_PLACEMENT_3D('',#3525,#2842,#2843);
#2530=AXIS2_PLACEMENT_3D('',#3527,#2844,#2845);
#2531=AXIS2_PLACEMENT_3D('',#3530,#2847,#2848);
#2532=AXIS2_PLACEMENT_3D('',#3531,#2849,#2850);
#2533=AXIS2_PLACEMENT_3D('',#3532,#2851,#2852);
#2534=AXIS2_PLACEMENT_3D('',#3533,#2853,#2854);
#2535=AXIS2_PLACEMENT_3D('',#3534,#2855,#2856);
#2536=AXIS2_PLACEMENT_3D('',#3535,#2857,#2858);
#2537=AXIS2_PLACEMENT_3D('',#3536,#2859,#2860);
#2538=AXIS2_PLACEMENT_3D('',#3537,#2861,#2862);
#2539=AXIS2_PLACEMENT_3D('',#3538,#2863,#2864);
#2540=AXIS2_PLACEMENT_3D('',#3539,#2865,#2866);
#2541=AXIS2_PLACEMENT_3D('',#3541,#2867,#2868);
#2542=AXIS2_PLACEMENT_3D('',#3544,#2870,#2871);
#2543=AXIS2_PLACEMENT_3D('',#3545,#2872,#2873);
#2544=AXIS2_PLACEMENT_3D('',#3547,#2874,#2875);
#2545=AXIS2_PLACEMENT_3D('',#3550,#2877,#2878);
#2546=AXIS2_PLACEMENT_3D('',#3551,#2879,#2880);
#2547=AXIS2_PLACEMENT_3D('',#3554,#2881,#2882);
#2548=AXIS2_PLACEMENT_3D('',#3558,#2884,#2885);
#2549=AXIS2_PLACEMENT_3D('',#3560,#2887,#2888);
#2550=AXIS2_PLACEMENT_3D('',#3563,#2889,#2890);
#2551=AXIS2_PLACEMENT_3D('',#3567,#2892,#2893);
#2552=AXIS2_PLACEMENT_3D('',#3569,#2895,#2896);
#2553=AXIS2_PLACEMENT_3D('',#3572,#2897,#2898);
#2554=AXIS2_PLACEMENT_3D('',#3576,#2900,#2901);
#2555=AXIS2_PLACEMENT_3D('',#3578,#2903,#2904);
#2556=AXIS2_PLACEMENT_3D('',#3581,#2905,#2906);
#2557=AXIS2_PLACEMENT_3D('',#3585,#2908,#2909);
#2558=AXIS2_PLACEMENT_3D('',#3587,#2911,#2912);
#2559=AXIS2_PLACEMENT_3D('',#3593,#2916,#2917);
#2560=AXIS2_PLACEMENT_3D('',#3599,#2921,#2922);
#2561=AXIS2_PLACEMENT_3D('',#3605,#2926,#2927);
#2562=AXIS2_PLACEMENT_3D('',#3611,#2931,#2932);
#2563=AXIS2_PLACEMENT_3D('',#3617,#2936,#2937);
#2564=AXIS2_PLACEMENT_3D('',#3623,#2941,#2942);
#2565=AXIS2_PLACEMENT_3D('',#3637,#2950,#2951);
#2566=AXIS2_PLACEMENT_3D('',#3639,#2952,#2953);
#2567=AXIS2_PLACEMENT_3D('',#3642,#2955,#2956);
#2568=AXIS2_PLACEMENT_3D('',#3643,#2957,#2958);
#2569=AXIS2_PLACEMENT_3D('',#3648,#2963,#2964);
#2570=AXIS2_PLACEMENT_3D('',#3654,#2968,#2969);
#2571=AXIS2_PLACEMENT_3D('',#3660,#2973,#2974);
#2572=AXIS2_PLACEMENT_3D('',#3666,#2978,#2979);
#2573=AXIS2_PLACEMENT_3D('',#3672,#2983,#2984);
#2574=AXIS2_PLACEMENT_3D('',#3678,#2988,#2989);
#2575=AXIS2_PLACEMENT_3D('',#3681,#2992,#2993);
#2576=AXIS2_PLACEMENT_3D('',#3687,#2997,#2998);
#2577=AXIS2_PLACEMENT_3D('',#3689,#2999,#3000);
#2578=AXIS2_PLACEMENT_3D('',#3691,#3002,#3003);
#2579=AXIS2_PLACEMENT_3D('',#3693,#3005,#3006);
#2580=AXIS2_PLACEMENT_3D('',#3701,#3011,#3012);
#2581=AXIS2_PLACEMENT_3D('',#3702,#3013,#3014);
#2582=AXIS2_PLACEMENT_3D('',#3703,#3015,#3016);
#2583=AXIS2_PLACEMENT_3D('',#3709,#3020,#3021);
#2584=AXIS2_PLACEMENT_3D('',#3715,#3025,#3026);
#2585=AXIS2_PLACEMENT_3D('',#3718,#3029,#3030);
#2586=AXIS2_PLACEMENT_3D('',#3721,#3033,#3034);
#2587=AXIS2_PLACEMENT_3D('',#3722,#3035,#3036);
#2588=AXIS2_PLACEMENT_3D('',#3723,#3037,#3038);
#2589=AXIS2_PLACEMENT_3D('',#3724,#3039,#3040);
#2590=AXIS2_PLACEMENT_3D('',#3725,#3041,#3042);
#2591=AXIS2_PLACEMENT_3D('',#4267,#3045,#3046);
#2592=AXIS2_PLACEMENT_3D('',#6477,#3047,#3048);
#2593=AXIS2_PLACEMENT_3D('',#7703,#3049,#3050);
#2594=AXIS2_PLACEMENT_3D('',#7705,#3051,#3052);
#2595=AXIS2_PLACEMENT_3D('',#7708,#3054,#3055);
#2596=AXIS2_PLACEMENT_3D('',#7709,#3056,#3057);
#2597=AXIS2_PLACEMENT_3D('',#7711,#3058,#3059);
#2598=AXIS2_PLACEMENT_3D('',#7714,#3061,#3062);
#2599=AXIS2_PLACEMENT_3D('',#7715,#3063,#3064);
#2600=AXIS2_PLACEMENT_3D('',#7717,#3065,#3066);
#2601=AXIS2_PLACEMENT_3D('',#7720,#3068,#3069);
#2602=AXIS2_PLACEMENT_3D('',#7723,#3070,#3071);
#2603=AXIS2_PLACEMENT_3D('',#7727,#3073,#3074);
#2604=AXIS2_PLACEMENT_3D('',#7729,#3076,#3077);
#2605=AXIS2_PLACEMENT_3D('',#7735,#3081,#3082);
#2606=AXIS2_PLACEMENT_3D('',#7741,#3086,#3087);
#2607=AXIS2_PLACEMENT_3D('',#7743,#3089,#3090);
#2608=AXIS2_PLACEMENT_3D('',#7745,#3092,#3093);
#2609=AXIS2_PLACEMENT_3D('',#7746,#3094,#3095);
#2610=AXIS2_PLACEMENT_3D('',#7747,#3096,#3097);
#2611=AXIS2_PLACEMENT_3D('',#7748,#3098,#3099);
#2612=AXIS2_PLACEMENT_3D('',#7773,#3100,#3101);
#2613=AXIS2_PLACEMENT_3D('',#9283,#3102,#3103);
#2614=AXIS2_PLACEMENT_3D('',#9284,#3104,#3105);
#2615=AXIS2_PLACEMENT_3D('',#9286,#3106,#3107);
#2616=AXIS2_PLACEMENT_3D('',#9289,#3109,#3110);
#2617=AXIS2_PLACEMENT_3D('',#9290,#3111,#3112);
#2618=AXIS2_PLACEMENT_3D('',#9299,#3117,#3118);
#2619=AXIS2_PLACEMENT_3D('',#9308,#3123,#3124);
#2620=AXIS2_PLACEMENT_3D('',#9317,#3129,#3130);
#2621=AXIS2_PLACEMENT_3D('',#9326,#3135,#3136);
#2622=AXIS2_PLACEMENT_3D('',#9335,#3141,#3142);
#2623=AXIS2_PLACEMENT_3D('',#9344,#3147,#3148);
#2624=AXIS2_PLACEMENT_3D('',#9353,#3153,#3154);
#2625=AXIS2_PLACEMENT_3D('',#9362,#3159,#3160);
#2626=AXIS2_PLACEMENT_3D('',#9371,#3165,#3166);
#2627=AXIS2_PLACEMENT_3D('',#9380,#3171,#3172);
#2628=AXIS2_PLACEMENT_3D('',#9389,#3177,#3178);
#2629=AXIS2_PLACEMENT_3D('',#9395,#3182,#3183);
#2630=AXIS2_PLACEMENT_3D('',#9401,#3187,#3188);
#2631=AXIS2_PLACEMENT_3D('',#9413,#3199,#3200);
#2632=AXIS2_PLACEMENT_3D('',#9414,#3201,#3202);
#2633=AXIS2_PLACEMENT_3D('',#9415,#3203,#3204);
#2634=AXIS2_PLACEMENT_3D('',#9427,#3215,#3216);
#2635=AXIS2_PLACEMENT_3D('',#9428,#3217,#3218);
#2636=AXIS2_PLACEMENT_3D('',#9429,#3219,#3220);
#2637=AXIS2_PLACEMENT_3D('',#9431,#3222,#3223);
#2638=AXIS2_PLACEMENT_3D('',#9432,#3224,#3225);
#2639=AXIS2_PLACEMENT_3D('',#9436,#3228,#3229);
#2640=AXIS2_PLACEMENT_3D('',#9438,#3231,#3232);
#2641=AXIS2_PLACEMENT_3D('',#9440,#3234,#3235);
#2642=AXIS2_PLACEMENT_3D('',#9441,#3236,#3237);
#2643=AXIS2_PLACEMENT_3D('',#9445,#3240,#3241);
#2644=AXIS2_PLACEMENT_3D('',#9447,#3243,#3244);
#2645=AXIS2_PLACEMENT_3D('',#9449,#3246,#3247);
#2646=AXIS2_PLACEMENT_3D('',#9450,#3248,#3249);
#2647=AXIS2_PLACEMENT_3D('',#9454,#3252,#3253);
#2648=AXIS2_PLACEMENT_3D('',#9456,#3255,#3256);
#2649=AXIS2_PLACEMENT_3D('',#9458,#3258,#3259);
#2650=AXIS2_PLACEMENT_3D('',#9459,#3260,#3261);
#2651=AXIS2_PLACEMENT_3D('',#9463,#3264,#3265);
#2652=AXIS2_PLACEMENT_3D('',#9465,#3267,#3268);
#2653=AXIS2_PLACEMENT_3D('',#9467,#3270,#3271);
#2654=AXIS2_PLACEMENT_3D('',#9468,#3272,#3273);
#2655=AXIS2_PLACEMENT_3D('',#9472,#3276,#3277);
#2656=AXIS2_PLACEMENT_3D('',#9474,#3279,#3280);
#2657=AXIS2_PLACEMENT_3D('',#9476,#3282,#3283);
#2658=AXIS2_PLACEMENT_3D('',#9477,#3284,#3285);
#2659=AXIS2_PLACEMENT_3D('',#9481,#3288,#3289);
#2660=AXIS2_PLACEMENT_3D('',#9483,#3291,#3292);
#2661=AXIS2_PLACEMENT_3D('',#9485,#3294,#3295);
#2662=AXIS2_PLACEMENT_3D('',#9486,#3296,#3297);
#2663=AXIS2_PLACEMENT_3D('',#9490,#3300,#3301);
#2664=AXIS2_PLACEMENT_3D('',#9492,#3303,#3304);
#2665=AXIS2_PLACEMENT_3D('',#9494,#3306,#3307);
#2666=AXIS2_PLACEMENT_3D('',#9495,#3308,#3309);
#2667=AXIS2_PLACEMENT_3D('',#9499,#3312,#3313);
#2668=AXIS2_PLACEMENT_3D('',#9501,#3315,#3316);
#2669=AXIS2_PLACEMENT_3D('',#9503,#3318,#3319);
#2670=AXIS2_PLACEMENT_3D('',#9504,#3320,#3321);
#2671=AXIS2_PLACEMENT_3D('',#9508,#3324,#3325);
#2672=AXIS2_PLACEMENT_3D('',#9510,#3327,#3328);
#2673=AXIS2_PLACEMENT_3D('',#9512,#3330,#3331);
#2674=AXIS2_PLACEMENT_3D('',#9513,#3332,#3333);
#2675=AXIS2_PLACEMENT_3D('',#9517,#3336,#3337);
#2676=AXIS2_PLACEMENT_3D('',#9519,#3339,#3340);
#2677=AXIS2_PLACEMENT_3D('',#9521,#3342,#3343);
#2678=AXIS2_PLACEMENT_3D('',#9522,#3344,#3345);
#2679=AXIS2_PLACEMENT_3D('',#9523,#3346,#3347);
#2680=AXIS2_PLACEMENT_3D('',#9525,#3348,#3349);
#2681=AXIS2_PLACEMENT_3D('',#9528,#3351,#3352);
#2682=AXIS2_PLACEMENT_3D('',#9529,#3353,#3354);
#2683=AXIS2_PLACEMENT_3D('',#9530,#3355,#3356);
#2684=AXIS2_PLACEMENT_3D('',#9531,#3357,#3358);
#2685=AXIS2_PLACEMENT_3D('',#9532,#3359,#3360);
#2686=AXIS2_PLACEMENT_3D('',#9534,#3361,#3362);
#2687=AXIS2_PLACEMENT_3D('',#9537,#3364,#3365);
#2688=AXIS2_PLACEMENT_3D('',#9538,#3366,#3367);
#2689=AXIS2_PLACEMENT_3D('',#9539,#3368,#3369);
#2690=AXIS2_PLACEMENT_3D('',#9540,#3370,#3371);
#2691=AXIS2_PLACEMENT_3D('',#9541,#3372,#3373);
#2692=AXIS2_PLACEMENT_3D('',#9542,#3374,#3375);
#2693=AXIS2_PLACEMENT_3D('',#9543,#3376,#3377);
#2694=AXIS2_PLACEMENT_3D('',#9544,#3378,#3379);
#2695=AXIS2_PLACEMENT_3D('',#9545,#3380,#3381);
#2696=DIRECTION('axis',(0.,0.,1.));
#2697=DIRECTION('refdir',(1.,0.,0.));
#2698=DIRECTION('axis',(0.,0.,1.));
#2699=DIRECTION('refdir',(1.,0.,0.));
#2700=DIRECTION('center_axis',(0.,0.,1.));
#2701=DIRECTION('ref_axis',(1.,0.,0.));
#2702=DIRECTION('center_axis',(0.,0.,1.));
#2703=DIRECTION('ref_axis',(1.,0.,0.));
#2704=DIRECTION('',(0.,0.,1.));
#2705=DIRECTION('center_axis',(0.,0.,1.));
#2706=DIRECTION('ref_axis',(1.,0.,0.));
#2707=DIRECTION('center_axis',(0.,0.,1.));
#2708=DIRECTION('ref_axis',(1.,0.,0.));
#2709=DIRECTION('center_axis',(0.,0.,1.));
#2710=DIRECTION('ref_axis',(1.,0.,0.));
#2711=DIRECTION('',(0.,0.,1.));
#2712=DIRECTION('center_axis',(0.,0.,1.));
#2713=DIRECTION('ref_axis',(1.,0.,0.));
#2714=DIRECTION('center_axis',(0.,0.,1.));
#2715=DIRECTION('ref_axis',(1.,0.,0.));
#2716=DIRECTION('center_axis',(0.,0.,1.));
#2717=DIRECTION('ref_axis',(1.,0.,0.));
#2718=DIRECTION('',(0.,0.,1.));
#2719=DIRECTION('center_axis',(0.,0.,1.));
#2720=DIRECTION('ref_axis',(1.,0.,0.));
#2721=DIRECTION('center_axis',(0.,0.,1.));
#2722=DIRECTION('ref_axis',(1.,0.,0.));
#2723=DIRECTION('center_axis',(0.,0.,1.));
#2724=DIRECTION('ref_axis',(1.,0.,0.));
#2725=DIRECTION('',(0.,0.,1.));
#2726=DIRECTION('center_axis',(0.,0.,1.));
#2727=DIRECTION('ref_axis',(1.,0.,0.));
#2728=DIRECTION('center_axis',(0.,0.,-1.));
#2729=DIRECTION('ref_axis',(-1.,0.,0.));
#2730=DIRECTION('center_axis',(0.,0.,-1.));
#2731=DIRECTION('ref_axis',(1.,0.,0.));
#2732=DIRECTION('',(0.,0.,-1.));
#2733=DIRECTION('center_axis',(0.,0.,-1.));
#2734=DIRECTION('ref_axis',(1.,0.,0.));
#2735=DIRECTION('',(0.,0.,-1.));
#2736=DIRECTION('center_axis',(0.,0.,-1.));
#2737=DIRECTION('ref_axis',(-1.,0.,0.));
#2738=DIRECTION('center_axis',(0.,0.,-1.));
#2739=DIRECTION('ref_axis',(-1.,0.,0.));
#2740=DIRECTION('',(0.,0.,-1.));
#2741=DIRECTION('center_axis',(0.,0.,-1.));
#2742=DIRECTION('ref_axis',(1.,0.,0.));
#2743=DIRECTION('',(0.,0.,-1.));
#2744=DIRECTION('center_axis',(0.,0.,-1.));
#2745=DIRECTION('ref_axis',(-1.,0.,0.));
#2746=DIRECTION('center_axis',(0.,0.,-1.));
#2747=DIRECTION('ref_axis',(-1.,0.,0.));
#2748=DIRECTION('',(0.,0.,-1.));
#2749=DIRECTION('center_axis',(0.,0.,-1.));
#2750=DIRECTION('ref_axis',(-1.,0.,0.));
#2751=DIRECTION('',(0.,0.,-1.));
#2752=DIRECTION('center_axis',(0.,0.,-1.));
#2753=DIRECTION('ref_axis',(-1.,0.,0.));
#2754=DIRECTION('center_axis',(0.,0.,-1.));
#2755=DIRECTION('ref_axis',(1.,0.,0.));
#2756=DIRECTION('',(0.,0.,-1.));
#2757=DIRECTION('center_axis',(0.,0.,-1.));
#2758=DIRECTION('ref_axis',(-1.,0.,0.));
#2759=DIRECTION('',(0.,0.,-1.));
#2760=DIRECTION('center_axis',(0.,1.,0.));
#2761=DIRECTION('ref_axis',(0.,0.,1.));
#2762=DIRECTION('',(1.,0.,0.));
#2763=DIRECTION('',(0.,0.,-1.));
#2764=DIRECTION('',(1.,0.,0.));
#2765=DIRECTION('',(0.,0.,-1.));
#2766=DIRECTION('center_axis',(-0.997701530936239,-0.0677617529841435,0.));
#2767=DIRECTION('ref_axis',(0.0677617529841435,-0.997701530936239,0.));
#2768=DIRECTION('',(-0.0677617529841435,0.997701530936239,0.));
#2769=DIRECTION('',(-0.0677617529841435,0.997701530936239,0.));
#2770=DIRECTION('',(0.,0.,-1.));
#2771=DIRECTION('center_axis',(0.,0.,-1.));
#2772=DIRECTION('ref_axis',(-1.,0.,0.));
#2773=DIRECTION('center_axis',(0.,0.,1.));
#2774=DIRECTION('ref_axis',(1.,0.,0.));
#2775=DIRECTION('center_axis',(0.,0.,1.));
#2776=DIRECTION('ref_axis',(1.,0.,0.));
#2777=DIRECTION('',(0.,0.,-1.));
#2778=DIRECTION('center_axis',(-1.,0.,0.));
#2779=DIRECTION('ref_axis',(0.,0.,1.));
#2780=DIRECTION('',(0.,0.,-1.));
#2781=DIRECTION('',(0.,1.,0.));
#2782=DIRECTION('',(0.,1.,0.));
#2783=DIRECTION('',(0.,0.,-1.));
#2784=DIRECTION('',(0.,1.,0.));
#2785=DIRECTION('',(0.,0.,-1.));
#2786=DIRECTION('',(0.,1.,0.));
#2787=DIRECTION('center_axis',(-0.456611069299162,0.889666415794974,0.));
#2788=DIRECTION('ref_axis',(-0.889666415794975,-0.456611069299162,0.));
#2789=DIRECTION('',(0.889666415794974,0.456611069299162,0.));
#2790=DIRECTION('',(0.889666415794974,0.456611069299162,0.));
#2791=DIRECTION('',(0.889666415794974,0.456611069299162,0.));
#2792=DIRECTION('',(0.889666415794974,0.456611069299162,0.));
#2793=DIRECTION('center_axis',(0.,0.,-1.));
#2794=DIRECTION('ref_axis',(0.999997864451694,-0.0020666620553607,0.));
#2795=DIRECTION('center_axis',(0.,0.,1.));
#2796=DIRECTION('ref_axis',(1.,0.,0.));
#2797=DIRECTION('center_axis',(0.,0.,1.));
#2798=DIRECTION('ref_axis',(1.,0.,0.));
#2799=DIRECTION('',(0.,0.,-1.));
#2800=DIRECTION('center_axis',(-1.,1.04083408558608E-15,0.));
#2801=DIRECTION('ref_axis',(-1.04083408558608E-15,-1.,0.));
#2802=DIRECTION('',(1.04083408558608E-15,1.,0.));
#2803=DIRECTION('',(1.04083408558608E-15,1.,0.));
#2804=DIRECTION('center_axis',(0.,1.,0.));
#2805=DIRECTION('ref_axis',(0.,0.,1.));
#2806=DIRECTION('',(0.,0.,-1.));
#2807=DIRECTION('',(1.,0.,0.));
#2808=DIRECTION('',(0.,0.,-1.));
#2809=DIRECTION('',(1.,0.,0.));
#2810=DIRECTION('center_axis',(-0.997701530936239,-0.0677617529841435,0.));
#2811=DIRECTION('ref_axis',(0.0677617529841435,-0.997701530936239,0.));
#2812=DIRECTION('',(-0.0677617529841435,0.997701530936239,0.));
#2813=DIRECTION('',(0.,0.,-1.));
#2814=DIRECTION('',(-0.0677617529841435,0.997701530936239,0.));
#2815=DIRECTION('center_axis',(0.,0.,-1.));
#2816=DIRECTION('ref_axis',(-1.,0.,0.));
#2817=DIRECTION('center_axis',(0.,0.,1.));
#2818=DIRECTION('ref_axis',(1.,0.,0.));
#2819=DIRECTION('center_axis',(0.,0.,1.));
#2820=DIRECTION('ref_axis',(1.,0.,0.));
#2821=DIRECTION('center_axis',(0.,0.,-1.));
#2822=DIRECTION('ref_axis',(1.,1.22464679914735E-16,0.));
#2823=DIRECTION('center_axis',(0.,0.,1.));
#2824=DIRECTION('ref_axis',(1.,0.,0.));
#2825=DIRECTION('center_axis',(0.,0.,1.));
#2826=DIRECTION('ref_axis',(1.,0.,0.));
#2827=DIRECTION('center_axis',(0.,0.,-1.));
#2828=DIRECTION('ref_axis',(0.999997864451694,-0.00206666205536139,0.));
#2829=DIRECTION('center_axis',(0.,0.,1.));
#2830=DIRECTION('ref_axis',(1.,0.,0.));
#2831=DIRECTION('',(0.,0.,-1.));
#2832=DIRECTION('center_axis',(0.,0.,1.));
#2833=DIRECTION('ref_axis',(1.,0.,0.));
#2834=DIRECTION('center_axis',(-1.,1.04083408558608E-15,0.));
#2835=DIRECTION('ref_axis',(-1.04083408558608E-15,-1.,0.));
#2836=DIRECTION('',(1.04083408558608E-15,1.,0.));
#2837=DIRECTION('',(1.04083408558608E-15,1.,0.));
#2838=DIRECTION('center_axis',(0.,0.,1.));
#2839=DIRECTION('ref_axis',(1.,0.,0.));
#2840=DIRECTION('center_axis',(0.,0.,1.));
#2841=DIRECTION('ref_axis',(1.,0.,0.));
#2842=DIRECTION('center_axis',(0.,0.,-1.));
#2843=DIRECTION('ref_axis',(0.999999985346409,-0.000171193403699097,0.));
#2844=DIRECTION('center_axis',(0.,0.,1.));
#2845=DIRECTION('ref_axis',(1.,0.,0.));
#2846=DIRECTION('',(0.,0.,1.));
#2847=DIRECTION('center_axis',(0.,0.,1.));
#2848=DIRECTION('ref_axis',(1.,0.,0.));
#2849=DIRECTION('center_axis',(0.,0.,1.));
#2850=DIRECTION('ref_axis',(1.,0.,0.));
#2851=DIRECTION('center_axis',(0.,0.,1.));
#2852=DIRECTION('ref_axis',(1.,0.,0.));
#2853=DIRECTION('center_axis',(0.,0.,1.));
#2854=DIRECTION('ref_axis',(1.,0.,0.));
#2855=DIRECTION('center_axis',(0.,0.,-1.));
#2856=DIRECTION('ref_axis',(1.,0.,0.));
#2857=DIRECTION('center_axis',(0.,0.,-1.));
#2858=DIRECTION('ref_axis',(-1.,0.,0.));
#2859=DIRECTION('center_axis',(0.,0.,1.));
#2860=DIRECTION('ref_axis',(1.,0.,0.));
#2861=DIRECTION('center_axis',(0.,0.,1.));
#2862=DIRECTION('ref_axis',(1.,0.,0.));
#2863=DIRECTION('axis',(0.,0.,1.));
#2864=DIRECTION('refdir',(1.,0.,0.));
#2865=DIRECTION('center_axis',(0.,0.,1.));
#2866=DIRECTION('ref_axis',(1.,0.,0.));
#2867=DIRECTION('center_axis',(0.,0.,-1.));
#2868=DIRECTION('ref_axis',(-1.,0.,0.));
#2869=DIRECTION('',(0.,0.,1.));
#2870=DIRECTION('center_axis',(0.,0.,1.));
#2871=DIRECTION('ref_axis',(1.,0.,0.));
#2872=DIRECTION('center_axis',(0.,0.,1.));
#2873=DIRECTION('ref_axis',(1.,0.,0.));
#2874=DIRECTION('center_axis',(0.,0.,1.));
#2875=DIRECTION('ref_axis',(1.,0.,0.));
#2876=DIRECTION('',(0.,0.,1.));
#2877=DIRECTION('center_axis',(0.,0.,-1.));
#2878=DIRECTION('ref_axis',(-1.,0.,0.));
#2879=DIRECTION('center_axis',(0.,0.,-1.));
#2880=DIRECTION('ref_axis',(-1.,0.,0.));
#2881=DIRECTION('center_axis',(0.,0.,1.));
#2882=DIRECTION('ref_axis',(-1.,0.,0.));
#2883=DIRECTION('',(0.,0.,-1.));
#2884=DIRECTION('center_axis',(0.,0.,1.));
#2885=DIRECTION('ref_axis',(-1.,0.,0.));
#2886=DIRECTION('',(0.,0.,-1.));
#2887=DIRECTION('center_axis',(0.,0.,1.));
#2888=DIRECTION('ref_axis',(1.,0.,0.));
#2889=DIRECTION('center_axis',(0.,0.,1.));
#2890=DIRECTION('ref_axis',(-1.,8.67361737988404E-16,0.));
#2891=DIRECTION('',(0.,0.,-1.));
#2892=DIRECTION('center_axis',(0.,0.,1.));
#2893=DIRECTION('ref_axis',(-1.,8.67361737988404E-16,0.));
#2894=DIRECTION('',(0.,0.,1.));
#2895=DIRECTION('center_axis',(0.,0.,1.));
#2896=DIRECTION('ref_axis',(1.,0.,0.));
#2897=DIRECTION('center_axis',(0.,0.,-1.));
#2898=DIRECTION('ref_axis',(-1.,0.,0.));
#2899=DIRECTION('',(0.,0.,-1.));
#2900=DIRECTION('center_axis',(0.,0.,-1.));
#2901=DIRECTION('ref_axis',(-1.,0.,0.));
#2902=DIRECTION('',(0.,0.,1.));
#2903=DIRECTION('center_axis',(0.,0.,-1.));
#2904=DIRECTION('ref_axis',(-1.,0.,0.));
#2905=DIRECTION('center_axis',(0.,0.,1.));
#2906=DIRECTION('ref_axis',(-1.,0.,0.));
#2907=DIRECTION('',(0.,0.,-1.));
#2908=DIRECTION('center_axis',(0.,0.,1.));
#2909=DIRECTION('ref_axis',(-1.,0.,0.));
#2910=DIRECTION('',(0.,0.,-1.));
#2911=DIRECTION('center_axis',(0.537299608346827,0.843391445812884,0.));
#2912=DIRECTION('ref_axis',(-0.843391445812884,0.537299608346827,0.));
#2913=DIRECTION('',(0.843391445812883,-0.537299608346827,0.));
#2914=DIRECTION('',(0.843391445812883,-0.537299608346827,0.));
#2915=DIRECTION('',(0.,0.,-1.));
#2916=DIRECTION('center_axis',(-0.707106781186552,0.707106781186543,0.));
#2917=DIRECTION('ref_axis',(-0.707106781186543,-0.707106781186552,0.));
#2918=DIRECTION('',(0.707106781186543,0.707106781186552,0.));
#2919=DIRECTION('',(0.707106781186543,0.707106781186552,0.));
#2920=DIRECTION('',(0.,0.,-1.));
#2921=DIRECTION('center_axis',(0.707106781186547,0.707106781186548,0.));
#2922=DIRECTION('ref_axis',(-0.707106781186548,0.707106781186547,0.));
#2923=DIRECTION('',(0.707106781186548,-0.707106781186547,0.));
#2924=DIRECTION('',(0.707106781186548,-0.707106781186547,0.));
#2925=DIRECTION('',(0.,0.,-1.));
#2926=DIRECTION('center_axis',(0.965925826289068,0.258819045102523,0.));
#2927=DIRECTION('ref_axis',(-0.258819045102523,0.965925826289068,0.));
#2928=DIRECTION('',(0.258819045102523,-0.965925826289068,0.));
#2929=DIRECTION('',(0.258819045102523,-0.965925826289068,0.));
#2930=DIRECTION('',(0.,0.,-1.));
#2931=DIRECTION('center_axis',(-0.707106781186541,0.707106781186554,0.));
#2932=DIRECTION('ref_axis',(-0.707106781186554,-0.707106781186541,0.));
#2933=DIRECTION('',(0.707106781186554,0.707106781186541,0.));
#2934=DIRECTION('',(0.707106781186554,0.707106781186541,0.));
#2935=DIRECTION('',(0.,0.,-1.));
#2936=DIRECTION('center_axis',(0.707106781186545,0.70710678118655,0.));
#2937=DIRECTION('ref_axis',(-0.70710678118655,0.707106781186545,0.));
#2938=DIRECTION('',(0.70710678118655,-0.707106781186545,0.));
#2939=DIRECTION('',(0.70710678118655,-0.707106781186545,0.));
#2940=DIRECTION('',(0.,0.,-1.));
#2941=DIRECTION('center_axis',(-0.707106781186549,0.707106781186546,0.));
#2942=DIRECTION('ref_axis',(-0.707106781186546,-0.707106781186549,0.));
#2943=DIRECTION('',(0.707106781186546,0.707106781186549,0.));
#2944=DIRECTION('',(0.707106781186546,0.707106781186549,0.));
#2945=DIRECTION('',(0.,0.,-1.));
#2946=DIRECTION('',(0.707106781186546,0.707106781186549,0.));
#2947=DIRECTION('',(0.,0.,-1.));
#2948=DIRECTION('',(0.707106781186546,0.707106781186549,0.));
#2949=DIRECTION('',(0.,0.,-1.));
#2950=DIRECTION('center_axis',(0.,0.,1.));
#2951=DIRECTION('ref_axis',(-0.99412594534969,0.10822940812268,0.));
#2952=DIRECTION('center_axis',(0.,0.,1.));
#2953=DIRECTION('ref_axis',(-1.,0.,0.));
#2954=DIRECTION('',(0.,0.,1.));
#2955=DIRECTION('center_axis',(0.,0.,1.));
#2956=DIRECTION('ref_axis',(-1.,0.,0.));
#2957=DIRECTION('center_axis',(-0.707106781186546,-0.707106781186549,0.));
#2958=DIRECTION('ref_axis',(0.707106781186549,-0.707106781186546,0.));
#2959=DIRECTION('',(-0.707106781186549,0.707106781186546,0.));
#2960=DIRECTION('',(0.,0.,-1.));
#2961=DIRECTION('',(-0.707106781186549,0.707106781186546,0.));
#2962=DIRECTION('',(0.,0.,-1.));
#2963=DIRECTION('center_axis',(0.537299608346827,0.843391445812884,0.));
#2964=DIRECTION('ref_axis',(-0.843391445812884,0.537299608346827,0.));
#2965=DIRECTION('',(0.843391445812883,-0.537299608346827,0.));
#2966=DIRECTION('',(0.,0.,-1.));
#2967=DIRECTION('',(0.843391445812883,-0.537299608346827,0.));
#2968=DIRECTION('center_axis',(-0.707106781186552,0.707106781186543,0.));
#2969=DIRECTION('ref_axis',(-0.707106781186543,-0.707106781186552,0.));
#2970=DIRECTION('',(0.707106781186543,0.707106781186552,0.));
#2971=DIRECTION('',(0.,0.,-1.));
#2972=DIRECTION('',(0.707106781186543,0.707106781186552,0.));
#2973=DIRECTION('center_axis',(0.707106781186547,0.707106781186548,0.));
#2974=DIRECTION('ref_axis',(-0.707106781186548,0.707106781186547,0.));
#2975=DIRECTION('',(0.707106781186548,-0.707106781186547,0.));
#2976=DIRECTION('',(0.,0.,-1.));
#2977=DIRECTION('',(0.707106781186548,-0.707106781186547,0.));
#2978=DIRECTION('center_axis',(0.965925826289068,0.258819045102523,0.));
#2979=DIRECTION('ref_axis',(-0.258819045102523,0.965925826289068,0.));
#2980=DIRECTION('',(0.258819045102523,-0.965925826289068,0.));
#2981=DIRECTION('',(0.,0.,-1.));
#2982=DIRECTION('',(0.258819045102523,-0.965925826289068,0.));
#2983=DIRECTION('center_axis',(-0.707106781186541,0.707106781186554,0.));
#2984=DIRECTION('ref_axis',(-0.707106781186554,-0.707106781186541,0.));
#2985=DIRECTION('',(0.707106781186554,0.707106781186541,0.));
#2986=DIRECTION('',(0.,0.,-1.));
#2987=DIRECTION('',(0.707106781186554,0.707106781186541,0.));
#2988=DIRECTION('center_axis',(0.707106781186545,0.70710678118655,0.));
#2989=DIRECTION('ref_axis',(-0.70710678118655,0.707106781186545,0.));
#2990=DIRECTION('',(0.70710678118655,-0.707106781186545,0.));
#2991=DIRECTION('',(0.70710678118655,-0.707106781186545,0.));
#2992=DIRECTION('center_axis',(-0.707106781186546,-0.707106781186549,0.));
#2993=DIRECTION('ref_axis',(0.707106781186549,-0.707106781186546,0.));
#2994=DIRECTION('',(-0.707106781186549,0.707106781186546,0.));
#2995=DIRECTION('',(0.,0.,1.));
#2996=DIRECTION('',(-0.707106781186549,0.707106781186546,0.));
#2997=DIRECTION('center_axis',(0.,0.,-1.));
#2998=DIRECTION('ref_axis',(-1.,0.,0.));
#2999=DIRECTION('center_axis',(0.,0.,1.));
#3000=DIRECTION('ref_axis',(-1.,0.,0.));
#3001=DIRECTION('',(0.965925826289068,-0.258819045102521,0.));
#3002=DIRECTION('center_axis',(0.,0.,-1.));
#3003=DIRECTION('ref_axis',(-1.,0.,0.));
#3004=DIRECTION('',(0.965925826289068,-0.258819045102521,0.));
#3005=DIRECTION('center_axis',(0.258819045102521,0.965925826289068,0.));
#3006=DIRECTION('ref_axis',(-0.965925826289068,0.258819045102521,0.));
#3007=DIRECTION('',(0.965925826289068,-0.258819045102521,0.));
#3008=DIRECTION('',(0.,0.,1.));
#3009=DIRECTION('',(0.965925826289068,-0.258819045102521,0.));
#3010=DIRECTION('',(0.,0.,1.));
#3011=DIRECTION('center_axis',(0.,0.,1.));
#3012=DIRECTION('ref_axis',(-0.99412594534969,0.10822940812268,0.));
#3013=DIRECTION('center_axis',(0.,0.,1.));
#3014=DIRECTION('ref_axis',(-1.,0.,0.));
#3015=DIRECTION('center_axis',(0.707106781186548,-0.707106781186547,0.));
#3016=DIRECTION('ref_axis',(0.,0.,-1.));
#3017=DIRECTION('',(0.707106781186547,0.707106781186548,0.));
#3018=DIRECTION('',(0.,0.,-1.));
#3019=DIRECTION('',(0.707106781186547,0.707106781186548,0.));
#3020=DIRECTION('center_axis',(0.707106781186549,-0.707106781186546,0.));
#3021=DIRECTION('ref_axis',(0.,0.,-1.));
#3022=DIRECTION('',(0.707106781186546,0.707106781186549,0.));
#3023=DIRECTION('',(0.,0.,-1.));
#3024=DIRECTION('',(0.707106781186546,0.707106781186549,0.));
#3025=DIRECTION('center_axis',(-0.707106781186546,-0.707106781186549,0.));
#3026=DIRECTION('ref_axis',(0.707106781186549,-0.707106781186546,0.));
#3027=DIRECTION('',(-0.707106781186549,0.707106781186546,0.));
#3028=DIRECTION('',(-0.707106781186549,0.707106781186546,0.));
#3029=DIRECTION('center_axis',(-0.707106781186546,-0.707106781186549,0.));
#3030=DIRECTION('ref_axis',(0.707106781186549,-0.707106781186546,0.));
#3031=DIRECTION('',(-0.707106781186549,0.707106781186546,0.));
#3032=DIRECTION('',(-0.707106781186549,0.707106781186546,0.));
#3033=DIRECTION('center_axis',(0.,0.,-1.));
#3034=DIRECTION('ref_axis',(-1.,0.,0.));
#3035=DIRECTION('center_axis',(0.,0.,-1.));
#3036=DIRECTION('ref_axis',(-1.,0.,0.));
#3037=DIRECTION('center_axis',(0.,0.,1.));
#3038=DIRECTION('ref_axis',(1.,0.,0.));
#3039=DIRECTION('center_axis',(0.,0.,1.));
#3040=DIRECTION('ref_axis',(1.,0.,0.));
#3041=DIRECTION('axis',(0.,0.,1.));
#3042=DIRECTION('refdir',(1.,0.,0.));
#3043=DIRECTION('',(-0.37576669481491,-0.860797132775134,0.34326037824658));
#3044=DIRECTION('',(-0.319221716607877,-0.41191406004893,0.853477769353091));
#3045=DIRECTION('center_axis',(0.405557992046095,0.691428751056098,-0.597870385033866));
#3046=DIRECTION('ref_axis',(-0.0717210395256331,-0.627988322886608,-0.774910807001314));
#3047=DIRECTION('center_axis',(0.421321917352423,0.692775741612449,-0.58527738192399));
#3048=DIRECTION('ref_axis',(0.0676843725596094,0.619533124468324,0.782047014825661));
#3049=DIRECTION('center_axis',(-0.499999999999995,0.866025403784442,0.));
#3050=DIRECTION('ref_axis',(-0.866025403784442,-0.499999999999995,0.));
#3051=DIRECTION('center_axis',(0.499999999999995,-0.866025403784442,0.));
#3052=DIRECTION('ref_axis',(0.866025403784442,0.499999999999995,0.));
#3053=DIRECTION('',(0.499999999999995,-0.866025403784442,0.));
#3054=DIRECTION('center_axis',(0.499999999999995,-0.866025403784442,0.));
#3055=DIRECTION('ref_axis',(0.866025403784442,0.499999999999995,0.));
#3056=DIRECTION('center_axis',(0.,0.,-1.));
#3057=DIRECTION('ref_axis',(-1.,0.,0.));
#3058=DIRECTION('center_axis',(0.,0.,1.));
#3059=DIRECTION('ref_axis',(1.,0.,0.));
#3060=DIRECTION('',(0.,0.,-1.));
#3061=DIRECTION('center_axis',(0.,0.,1.));
#3062=DIRECTION('ref_axis',(1.,0.,0.));
#3063=DIRECTION('center_axis',(0.,0.,-1.));
#3064=DIRECTION('ref_axis',(-1.,0.,0.));
#3065=DIRECTION('center_axis',(0.,0.,1.));
#3066=DIRECTION('ref_axis',(1.,0.,0.));
#3067=DIRECTION('',(0.,0.,1.));
#3068=DIRECTION('center_axis',(0.,0.,1.));
#3069=DIRECTION('ref_axis',(1.,0.,0.));
#3070=DIRECTION('center_axis',(0.,0.,-1.));
#3071=DIRECTION('ref_axis',(-1.,0.,0.));
#3072=DIRECTION('',(0.,0.,-1.));
#3073=DIRECTION('center_axis',(0.,0.,-1.));
#3074=DIRECTION('ref_axis',(-1.,0.,0.));
#3075=DIRECTION('',(0.,0.,-1.));
#3076=DIRECTION('center_axis',(0.866025403784442,0.499999999999995,0.));
#3077=DIRECTION('ref_axis',(-0.499999999999995,0.866025403784442,0.));
#3078=DIRECTION('',(0.,0.,-1.));
#3079=DIRECTION('',(0.499999999999995,-0.866025403784442,0.));
#3080=DIRECTION('',(0.499999999999995,-0.866025403784442,0.));
#3081=DIRECTION('center_axis',(0.866025403784442,0.499999999999995,0.));
#3082=DIRECTION('ref_axis',(-0.499999999999995,0.866025403784442,0.));
#3083=DIRECTION('',(0.499999999999995,-0.866025403784442,0.));
#3084=DIRECTION('',(0.,0.,-1.));
#3085=DIRECTION('',(0.499999999999995,-0.866025403784442,0.));
#3086=DIRECTION('center_axis',(0.,0.,-1.));
#3087=DIRECTION('ref_axis',(-1.,0.,0.));
#3088=DIRECTION('',(-0.866025403784442,-0.499999999999995,0.));
#3089=DIRECTION('center_axis',(0.,0.,-1.));
#3090=DIRECTION('ref_axis',(-1.,0.,0.));
#3091=DIRECTION('',(-0.866025403784442,-0.499999999999995,0.));
#3092=DIRECTION('center_axis',(0.,0.,1.));
#3093=DIRECTION('ref_axis',(1.,0.,0.));
#3094=DIRECTION('center_axis',(0.,0.,1.));
#3095=DIRECTION('ref_axis',(1.,0.,0.));
#3096=DIRECTION('center_axis',(0.499999999999995,-0.866025403784442,0.));
#3097=DIRECTION('ref_axis',(0.866025403784442,0.499999999999995,0.));
#3098=DIRECTION('center_axis',(0.499999999999995,-0.866025403784442,0.));
#3099=DIRECTION('ref_axis',(0.866025403784442,0.499999999999995,0.));
#3100=DIRECTION('center_axis',(0.368362767830729,0.663796275596578,-0.65090965254803));
#3101=DIRECTION('ref_axis',(-7.6388663671058E-18,0.700142154364021,0.714003475959681));
#3102=DIRECTION('axis',(0.,0.,1.));
#3103=DIRECTION('refdir',(1.,0.,0.));
#3104=DIRECTION('center_axis',(0.,0.,1.));
#3105=DIRECTION('ref_axis',(1.,0.,0.));
#3106=DIRECTION('center_axis',(0.,0.,-1.));
#3107=DIRECTION('ref_axis',(-1.,0.,0.));
#3108=DIRECTION('',(0.,0.,1.));
#3109=DIRECTION('center_axis',(0.,0.,-1.));
#3110=DIRECTION('ref_axis',(-1.,0.,0.));
#3111=DIRECTION('center_axis',(0.,-1.,0.));
#3112=DIRECTION('ref_axis',(0.,0.,-1.));
#3113=DIRECTION('',(0.,0.,1.));
#3114=DIRECTION('',(-1.,-1.22464679914735E-16,0.));
#3115=DIRECTION('',(0.,0.,1.));
#3116=DIRECTION('',(-1.,0.,0.));
#3117=DIRECTION('center_axis',(0.,-1.,0.));
#3118=DIRECTION('ref_axis',(0.,0.,-1.));
#3119=DIRECTION('',(0.,0.,1.));
#3120=DIRECTION('',(-1.,0.,0.));
#3121=DIRECTION('',(0.,0.,1.));
#3122=DIRECTION('',(-1.,-1.22464679914735E-16,0.));
#3123=DIRECTION('center_axis',(0.,-1.,0.));
#3124=DIRECTION('ref_axis',(0.,0.,-1.));
#3125=DIRECTION('',(0.,0.,1.));
#3126=DIRECTION('',(-1.,0.,0.));
#3127=DIRECTION('',(0.,0.,1.));
#3128=DIRECTION('',(-1.,-1.22464679914735E-16,0.));
#3129=DIRECTION('center_axis',(0.,-1.,0.));
#3130=DIRECTION('ref_axis',(0.,0.,-1.));
#3131=DIRECTION('',(0.,0.,1.));
#3132=DIRECTION('',(-1.,0.,0.));
#3133=DIRECTION('',(0.,0.,1.));
#3134=DIRECTION('',(-1.,-1.22464679914735E-16,0.));
#3135=DIRECTION('center_axis',(0.,-1.,0.));
#3136=DIRECTION('ref_axis',(0.,0.,-1.));
#3137=DIRECTION('',(0.,0.,1.));
#3138=DIRECTION('',(-1.,0.,0.));
#3139=DIRECTION('',(0.,0.,1.));
#3140=DIRECTION('',(-1.,-1.22464679914735E-16,0.));
#3141=DIRECTION('center_axis',(0.,-1.,0.));
#3142=DIRECTION('ref_axis',(0.,0.,-1.));
#3143=DIRECTION('',(0.,0.,1.));
#3144=DIRECTION('',(-1.,0.,0.));
#3145=DIRECTION('',(0.,0.,1.));
#3146=DIRECTION('',(-1.,-1.22464679914735E-16,0.));
#3147=DIRECTION('center_axis',(0.,-1.,0.));
#3148=DIRECTION('ref_axis',(0.,0.,-1.));
#3149=DIRECTION('',(0.,0.,1.));
#3150=DIRECTION('',(-1.,0.,0.));
#3151=DIRECTION('',(0.,0.,1.));
#3152=DIRECTION('',(-1.,-1.22464679914735E-16,0.));
#3153=DIRECTION('center_axis',(0.,-1.,0.));
#3154=DIRECTION('ref_axis',(0.,0.,-1.));
#3155=DIRECTION('',(0.,0.,1.));
#3156=DIRECTION('',(-1.,0.,0.));
#3157=DIRECTION('',(0.,0.,1.));
#3158=DIRECTION('',(-1.,-1.22464679914735E-16,0.));
#3159=DIRECTION('center_axis',(0.,-1.,0.));
#3160=DIRECTION('ref_axis',(0.,0.,-1.));
#3161=DIRECTION('',(0.,0.,1.));
#3162=DIRECTION('',(-1.,0.,0.));
#3163=DIRECTION('',(0.,0.,1.));
#3164=DIRECTION('',(-1.,-1.22464679914735E-16,0.));
#3165=DIRECTION('center_axis',(0.,-1.,0.));
#3166=DIRECTION('ref_axis',(0.,0.,-1.));
#3167=DIRECTION('',(-1.,0.,0.));
#3168=DIRECTION('',(0.,0.,1.));
#3169=DIRECTION('',(-1.,-1.22464679914735E-16,0.));
#3170=DIRECTION('',(0.,0.,-1.));
#3171=DIRECTION('center_axis',(0.,-1.,0.));
#3172=DIRECTION('ref_axis',(0.,0.,-1.));
#3173=DIRECTION('',(0.,0.,1.));
#3174=DIRECTION('',(-1.,0.,0.));
#3175=DIRECTION('',(0.,0.,-1.));
#3176=DIRECTION('',(-1.,-1.22464679914735E-16,0.));
#3177=DIRECTION('center_axis',(1.,0.,0.));
#3178=DIRECTION('ref_axis',(0.,0.,-1.));
#3179=DIRECTION('',(0.,-1.,0.));
#3180=DIRECTION('',(0.,0.,-1.));
#3181=DIRECTION('',(0.,-1.,0.));
#3182=DIRECTION('center_axis',(0.,-1.,0.));
#3183=DIRECTION('ref_axis',(0.,0.,-1.));
#3184=DIRECTION('',(-1.,0.,0.));
#3185=DIRECTION('',(0.,0.,1.));
#3186=DIRECTION('',(-1.,-1.22464679914735E-16,0.));
#3187=DIRECTION('center_axis',(0.,0.,-1.));
#3188=DIRECTION('ref_axis',(-1.,0.,0.));
#3189=DIRECTION('',(1.,0.,0.));
#3190=DIRECTION('',(1.,0.,0.));
#3191=DIRECTION('',(1.,0.,0.));
#3192=DIRECTION('',(1.,0.,0.));
#3193=DIRECTION('',(1.,0.,0.));
#3194=DIRECTION('',(1.,0.,0.));
#3195=DIRECTION('',(1.,0.,0.));
#3196=DIRECTION('',(1.,0.,0.));
#3197=DIRECTION('',(1.,0.,0.));
#3198=DIRECTION('',(1.,0.,0.));
#3199=DIRECTION('center_axis',(0.,0.,1.));
#3200=DIRECTION('ref_axis',(-1.,0.,0.));
#3201=DIRECTION('center_axis',(0.,0.,1.));
#3202=DIRECTION('ref_axis',(-1.,3.46944695195361E-15,0.));
#3203=DIRECTION('center_axis',(0.,0.,-1.));
#3204=DIRECTION('ref_axis',(-1.,0.,0.));
#3205=DIRECTION('',(-1.,0.,0.));
#3206=DIRECTION('',(-1.,0.,0.));
#3207=DIRECTION('',(-1.,0.,0.));
#3208=DIRECTION('',(-1.,0.,0.));
#3209=DIRECTION('',(-1.,0.,0.));
#3210=DIRECTION('',(-1.,0.,0.));
#3211=DIRECTION('',(-1.,0.,0.));
#3212=DIRECTION('',(-1.,0.,0.));
#3213=DIRECTION('',(-1.,0.,0.));
#3214=DIRECTION('',(-1.,0.,0.));
#3215=DIRECTION('center_axis',(0.,0.,-1.));
#3216=DIRECTION('ref_axis',(-1.,0.,0.));
#3217=DIRECTION('center_axis',(0.,0.,-1.));
#3218=DIRECTION('ref_axis',(-1.,0.,0.));
#3219=DIRECTION('center_axis',(0.,0.,1.));
#3220=DIRECTION('ref_axis',(1.,0.,0.));
#3221=DIRECTION('',(0.,0.,1.));
#3222=DIRECTION('center_axis',(0.,0.,1.));
#3223=DIRECTION('ref_axis',(-0.961769203083568,-0.273861278752579,0.));
#3224=DIRECTION('center_axis',(-1.,0.,0.));
#3225=DIRECTION('ref_axis',(0.,0.,1.));
#3226=DIRECTION('',(0.,-0.707106781186547,0.707106781186547));
#3227=DIRECTION('',(0.,0.707106781186548,0.707106781186548));
#3228=DIRECTION('center_axis',(0.,0.707106781186548,-0.707106781186548));
#3229=DIRECTION('ref_axis',(-1.,0.,0.));
#3230=DIRECTION('',(-0.577350269189626,-0.577350269189626,-0.577350269189626));
#3231=DIRECTION('center_axis',(-0.707106781186548,0.707106781186548,0.));
#3232=DIRECTION('ref_axis',(0.,0.,1.));
#3233=DIRECTION('',(-0.577350269189626,-0.577350269189626,0.577350269189626));
#3234=DIRECTION('center_axis',(0.,-0.707106781186548,-0.707106781186548));
#3235=DIRECTION('ref_axis',(1.,0.,0.));
#3236=DIRECTION('center_axis',(-1.,0.,0.));
#3237=DIRECTION('ref_axis',(0.,0.,1.));
#3238=DIRECTION('',(0.,-0.707106781186547,0.707106781186547));
#3239=DIRECTION('',(0.,0.707106781186548,0.707106781186548));
#3240=DIRECTION('center_axis',(0.,0.707106781186548,-0.707106781186548));
#3241=DIRECTION('ref_axis',(-1.,0.,0.));
#3242=DIRECTION('',(-0.577350269189626,-0.577350269189626,-0.577350269189626));
#3243=DIRECTION('center_axis',(-0.707106781186548,0.707106781186548,0.));
#3244=DIRECTION('ref_axis',(0.,0.,1.));
#3245=DIRECTION('',(-0.577350269189626,-0.577350269189626,0.577350269189626));
#3246=DIRECTION('center_axis',(0.,-0.707106781186548,-0.707106781186548));
#3247=DIRECTION('ref_axis',(1.,0.,0.));
#3248=DIRECTION('center_axis',(-1.,0.,0.));
#3249=DIRECTION('ref_axis',(0.,0.,1.));
#3250=DIRECTION('',(0.,-0.707106781186547,0.707106781186547));
#3251=DIRECTION('',(0.,0.707106781186548,0.707106781186548));
#3252=DIRECTION('center_axis',(0.,0.707106781186548,-0.707106781186548));
#3253=DIRECTION('ref_axis',(-1.,0.,0.));
#3254=DIRECTION('',(-0.577350269189626,-0.577350269189626,-0.577350269189626));
#3255=DIRECTION('center_axis',(-0.707106781186548,0.707106781186548,0.));
#3256=DIRECTION('ref_axis',(0.,0.,1.));
#3257=DIRECTION('',(-0.577350269189626,-0.577350269189626,0.577350269189626));
#3258=DIRECTION('center_axis',(0.,-0.707106781186548,-0.707106781186548));
#3259=DIRECTION('ref_axis',(1.,0.,0.));
#3260=DIRECTION('center_axis',(-1.,0.,0.));
#3261=DIRECTION('ref_axis',(0.,0.,1.));
#3262=DIRECTION('',(0.,-0.707106781186547,0.707106781186547));
#3263=DIRECTION('',(0.,0.707106781186548,0.707106781186548));
#3264=DIRECTION('center_axis',(0.,0.707106781186548,-0.707106781186548));
#3265=DIRECTION('ref_axis',(-1.,0.,0.));
#3266=DIRECTION('',(-0.577350269189626,-0.577350269189626,-0.577350269189626));
#3267=DIRECTION('center_axis',(-0.707106781186548,0.707106781186548,0.));
#3268=DIRECTION('ref_axis',(0.,0.,1.));
#3269=DIRECTION('',(-0.577350269189626,-0.577350269189626,0.577350269189626));
#3270=DIRECTION('center_axis',(0.,-0.707106781186548,-0.707106781186548));
#3271=DIRECTION('ref_axis',(1.,0.,0.));
#3272=DIRECTION('center_axis',(-1.,0.,0.));
#3273=DIRECTION('ref_axis',(0.,0.,1.));
#3274=DIRECTION('',(0.,-0.707106781186547,0.707106781186547));
#3275=DIRECTION('',(0.,0.707106781186548,0.707106781186548));
#3276=DIRECTION('center_axis',(0.,0.707106781186548,-0.707106781186548));
#3277=DIRECTION('ref_axis',(-1.,0.,0.));
#3278=DIRECTION('',(-0.577350269189626,-0.577350269189626,-0.577350269189626));
#3279=DIRECTION('center_axis',(-0.707106781186548,0.707106781186548,0.));
#3280=DIRECTION('ref_axis',(0.,0.,1.));
#3281=DIRECTION('',(-0.577350269189626,-0.577350269189626,0.577350269189626));
#3282=DIRECTION('center_axis',(0.,-0.707106781186548,-0.707106781186548));
#3283=DIRECTION('ref_axis',(1.,0.,0.));
#3284=DIRECTION('center_axis',(-1.,0.,0.));
#3285=DIRECTION('ref_axis',(0.,0.,1.));
#3286=DIRECTION('',(0.,-0.707106781186547,0.707106781186547));
#3287=DIRECTION('',(0.,0.707106781186548,0.707106781186548));
#3288=DIRECTION('center_axis',(0.,0.707106781186548,-0.707106781186548));
#3289=DIRECTION('ref_axis',(-1.,0.,0.));
#3290=DIRECTION('',(-0.577350269189626,-0.577350269189626,-0.577350269189626));
#3291=DIRECTION('center_axis',(-0.707106781186548,0.707106781186548,0.));
#3292=DIRECTION('ref_axis',(0.,0.,1.));
#3293=DIRECTION('',(-0.577350269189626,-0.577350269189626,0.577350269189626));
#3294=DIRECTION('center_axis',(0.,-0.707106781186548,-0.707106781186548));
#3295=DIRECTION('ref_axis',(1.,0.,0.));
#3296=DIRECTION('center_axis',(-1.,0.,0.));
#3297=DIRECTION('ref_axis',(0.,0.,1.));
#3298=DIRECTION('',(0.,-0.707106781186547,0.707106781186547));
#3299=DIRECTION('',(0.,0.707106781186548,0.707106781186548));
#3300=DIRECTION('center_axis',(0.,0.707106781186548,-0.707106781186548));
#3301=DIRECTION('ref_axis',(-1.,0.,0.));
#3302=DIRECTION('',(-0.577350269189626,-0.577350269189626,-0.577350269189626));
#3303=DIRECTION('center_axis',(-0.707106781186548,0.707106781186548,0.));
#3304=DIRECTION('ref_axis',(0.,0.,1.));
#3305=DIRECTION('',(-0.577350269189626,-0.577350269189626,0.577350269189626));
#3306=DIRECTION('center_axis',(0.,-0.707106781186548,-0.707106781186548));
#3307=DIRECTION('ref_axis',(1.,0.,0.));
#3308=DIRECTION('center_axis',(-1.,0.,0.));
#3309=DIRECTION('ref_axis',(0.,0.,1.));
#3310=DIRECTION('',(0.,-0.707106781186547,0.707106781186547));
#3311=DIRECTION('',(0.,0.707106781186548,0.707106781186548));
#3312=DIRECTION('center_axis',(0.,0.707106781186548,-0.707106781186548));
#3313=DIRECTION('ref_axis',(-1.,0.,0.));
#3314=DIRECTION('',(-0.577350269189626,-0.577350269189626,-0.577350269189626));
#3315=DIRECTION('center_axis',(-0.707106781186548,0.707106781186548,0.));
#3316=DIRECTION('ref_axis',(0.,0.,1.));
#3317=DIRECTION('',(-0.577350269189626,-0.577350269189626,0.577350269189626));
#3318=DIRECTION('center_axis',(0.,-0.707106781186548,-0.707106781186548));
#3319=DIRECTION('ref_axis',(1.,0.,0.));
#3320=DIRECTION('center_axis',(-1.,0.,0.));
#3321=DIRECTION('ref_axis',(0.,0.,1.));
#3322=DIRECTION('',(0.,-0.707106781186547,0.707106781186547));
#3323=DIRECTION('',(0.,0.707106781186548,0.707106781186548));
#3324=DIRECTION('center_axis',(0.,0.707106781186548,-0.707106781186548));
#3325=DIRECTION('ref_axis',(-1.,0.,0.));
#3326=DIRECTION('',(-0.577350269189626,-0.577350269189626,-0.577350269189626));
#3327=DIRECTION('center_axis',(-0.707106781186548,0.707106781186548,0.));
#3328=DIRECTION('ref_axis',(0.,0.,1.));
#3329=DIRECTION('',(-0.577350269189626,-0.577350269189626,0.577350269189626));
#3330=DIRECTION('center_axis',(0.,-0.707106781186548,-0.707106781186548));
#3331=DIRECTION('ref_axis',(1.,0.,0.));
#3332=DIRECTION('center_axis',(-1.,0.,0.));
#3333=DIRECTION('ref_axis',(0.,0.,1.));
#3334=DIRECTION('',(0.,-0.707106781186547,0.707106781186547));
#3335=DIRECTION('',(0.,0.707106781186548,0.707106781186548));
#3336=DIRECTION('center_axis',(0.,0.707106781186548,-0.707106781186548));
#3337=DIRECTION('ref_axis',(-1.,0.,0.));
#3338=DIRECTION('',(-0.577350269189626,-0.577350269189626,-0.577350269189626));
#3339=DIRECTION('center_axis',(-0.707106781186548,0.707106781186548,0.));
#3340=DIRECTION('ref_axis',(0.,0.,1.));
#3341=DIRECTION('',(-0.577350269189626,-0.577350269189626,0.577350269189626));
#3342=DIRECTION('center_axis',(0.,-0.707106781186548,-0.707106781186548));
#3343=DIRECTION('ref_axis',(1.,0.,0.));
#3344=DIRECTION('axis',(0.,0.,1.));
#3345=DIRECTION('refdir',(1.,0.,0.));
#3346=DIRECTION('center_axis',(0.,0.,-1.));
#3347=DIRECTION('ref_axis',(-1.,0.,0.));
#3348=DIRECTION('center_axis',(0.,0.,1.));
#3349=DIRECTION('ref_axis',(1.,0.,0.));
#3350=DIRECTION('',(0.,0.,1.));
#3351=DIRECTION('center_axis',(0.,0.,1.));
#3352=DIRECTION('ref_axis',(1.,0.,0.));
#3353=DIRECTION('center_axis',(0.,0.,1.));
#3354=DIRECTION('ref_axis',(1.,0.,0.));
#3355=DIRECTION('center_axis',(0.,0.,1.));
#3356=DIRECTION('ref_axis',(1.,0.,0.));
#3357=DIRECTION('axis',(0.,0.,1.));
#3358=DIRECTION('refdir',(1.,0.,0.));
#3359=DIRECTION('center_axis',(0.,0.,-1.));
#3360=DIRECTION('ref_axis',(-1.,0.,0.));
#3361=DIRECTION('center_axis',(0.,0.,1.));
#3362=DIRECTION('ref_axis',(1.,0.,0.));
#3363=DIRECTION('',(0.,0.,1.));
#3364=DIRECTION('center_axis',(0.,0.,1.));
#3365=DIRECTION('ref_axis',(1.,0.,0.));
#3366=DIRECTION('center_axis',(0.,0.,1.));
#3367=DIRECTION('ref_axis',(1.,0.,0.));
#3368=DIRECTION('center_axis',(0.,0.,1.));
#3369=DIRECTION('ref_axis',(1.,0.,0.));
#3370=DIRECTION('',(0.,0.,1.));
#3371=DIRECTION('',(1.,0.,0.));
#3372=DIRECTION('',(0.,0.,1.));
#3373=DIRECTION('',(1.,0.,0.));
#3374=DIRECTION('',(0.,0.,1.));
#3375=DIRECTION('',(1.,0.,0.));
#3376=DIRECTION('',(0.,0.,1.));
#3377=DIRECTION('',(1.,0.,0.));
#3378=DIRECTION('',(0.,0.,1.));
#3379=DIRECTION('',(1.,0.,0.));
#3380=DIRECTION('',(0.,0.,1.));
#3381=DIRECTION('',(1.,0.,0.));
#3382=CARTESIAN_POINT('',(0.,0.,0.));
#3383=CARTESIAN_POINT('',(0.,0.,0.));
#3384=CARTESIAN_POINT('Origin',(0.,0.,-4.5));
#3385=CARTESIAN_POINT('',(-1.25,-1.53080849893419E-16,3.));
#3386=CARTESIAN_POINT('Origin',(0.,0.,3.));
#3387=CARTESIAN_POINT('',(-1.25,-1.53080849893419E-16,4.));
#3388=CARTESIAN_POINT('',(-1.25,-1.53080849893419E-16,-4.5));
#3389=CARTESIAN_POINT('Origin',(0.,0.,4.));
#3390=CARTESIAN_POINT('Origin',(0.,0.,-4.5));
#3391=CARTESIAN_POINT('',(-1.25,-1.53080849893419E-16,-4.));
#3392=CARTESIAN_POINT('Origin',(0.,0.,-4.));
#3393=CARTESIAN_POINT('',(-1.25,-1.53080849893419E-16,-3.));
#3394=CARTESIAN_POINT('',(-1.25,-1.53080849893419E-16,-4.5));
#3395=CARTESIAN_POINT('Origin',(0.,0.,-3.));
#3396=CARTESIAN_POINT('Origin',(0.,-10.,-3.5));
#3397=CARTESIAN_POINT('',(-1.5,-10.,3.));
#3398=CARTESIAN_POINT('Origin',(0.,-10.,3.));
#3399=CARTESIAN_POINT('',(-1.5,-10.,3.5));
#3400=CARTESIAN_POINT('',(-1.5,-10.,-3.5));
#3401=CARTESIAN_POINT('Origin',(0.,-10.,3.5));
#3402=CARTESIAN_POINT('Origin',(0.,-10.,-3.5));
#3403=CARTESIAN_POINT('',(-1.5,-10.,-3.5));
#3404=CARTESIAN_POINT('Origin',(0.,-10.,-3.5));
#3405=CARTESIAN_POINT('',(-1.5,-10.,-3.));
#3406=CARTESIAN_POINT('',(-1.5,-10.,-3.5));
#3407=CARTESIAN_POINT('Origin',(0.,-10.,-3.));
#3408=CARTESIAN_POINT('Origin',(44.4833207897487,-57.1694465350419,4.));
#3409=CARTESIAN_POINT('',(0.889666415794979,-79.5433889307008,3.));
#3410=CARTESIAN_POINT('',(-4.01080902459558,-50.1466711898151,3.));
#3411=CARTESIAN_POINT('Origin',(44.4833207897487,-57.1694465350419,3.));
#3412=CARTESIAN_POINT('',(0.889666415794979,-79.5433889307008,-3.));
#3413=CARTESIAN_POINT('',(0.889666415794979,-79.5433889307008,3.));
#3414=CARTESIAN_POINT('',(-4.01080902459558,-50.1466711898151,-3.));
#3415=CARTESIAN_POINT('Origin',(44.4833207897487,-57.1694465350419,-3.));
#3416=CARTESIAN_POINT('',(-4.01080902459558,-50.1466711898151,3.));
#3417=CARTESIAN_POINT('Origin',(44.4833207897487,-57.1694465350419,4.));
#3418=CARTESIAN_POINT('',(5.33799849476985,-77.260333584205,4.));
#3419=CARTESIAN_POINT('',(0.935261287824902,-50.8792546765288,4.));
#3420=CARTESIAN_POINT('Origin',(44.4833207897487,-57.1694465350419,4.));
#3421=CARTESIAN_POINT('',(5.33799849476985,-77.260333584205,3.));
#3422=CARTESIAN_POINT('',(5.33799849476985,-77.260333584205,4.));
#3423=CARTESIAN_POINT('',(0.935261287824902,-50.8792546765288,3.));
#3424=CARTESIAN_POINT('Origin',(44.4833207897487,-57.1694465350419,3.));
#3425=CARTESIAN_POINT('',(0.935261287824902,-50.8792546765288,4.));
#3426=CARTESIAN_POINT('Origin',(44.4833207897487,-57.1694465350419,4.));
#3427=CARTESIAN_POINT('',(6.93889390390723E-15,-80.,4.));
#3428=CARTESIAN_POINT('',(-5.,-50.0000000000001,4.));
#3429=CARTESIAN_POINT('Origin',(44.4833207897487,-57.1694465350419,4.));
#3430=CARTESIAN_POINT('',(-5.,-50.0000000000001,-4.));
#3431=CARTESIAN_POINT('',(-5.,-50.0000000000001,4.));
#3432=CARTESIAN_POINT('',(6.93889390390723E-15,-80.,-4.));
#3433=CARTESIAN_POINT('Origin',(44.4833207897487,-57.1694465350419,-4.));
#3434=CARTESIAN_POINT('',(6.93889390390723E-15,-80.,4.));
#3435=CARTESIAN_POINT('Origin',(44.4833207897487,-57.1694465350419,4.));
#3436=CARTESIAN_POINT('',(5.33799849476985,-77.260333584205,-3.));
#3437=CARTESIAN_POINT('',(0.935261287824902,-50.8792546765288,-3.));
#3438=CARTESIAN_POINT('Origin',(44.4833207897487,-57.1694465350419,-3.));
#3439=CARTESIAN_POINT('',(5.33799849476985,-77.260333584205,-4.));
#3440=CARTESIAN_POINT('',(5.33799849476985,-77.260333584205,4.));
#3441=CARTESIAN_POINT('',(0.935261287824902,-50.8792546765288,-4.));
#3442=CARTESIAN_POINT('Origin',(44.4833207897487,-57.1694465350419,-4.));
#3443=CARTESIAN_POINT('',(0.935261287824902,-50.8792546765288,4.));
#3444=CARTESIAN_POINT('Origin',(1.00000000000001,-14.5540683672724,4.));
#3445=CARTESIAN_POINT('',(1.00000000000001,-14.5540683672724,-3.));
#3446=CARTESIAN_POINT('',(6.00000000000001,-14.5540683672724,-3.));
#3447=CARTESIAN_POINT('',(1.00000000000001,-14.5540683672724,-3.));
#3448=CARTESIAN_POINT('',(1.00000000000001,-14.5540683672724,-4.));
#3449=CARTESIAN_POINT('',(1.00000000000001,-14.5540683672724,4.));
#3450=CARTESIAN_POINT('',(6.00000000000001,-14.5540683672724,-4.));
#3451=CARTESIAN_POINT('',(1.00000000000001,-14.5540683672724,-4.));
#3452=CARTESIAN_POINT('',(6.00000000000001,-14.5540683672724,4.));
#3453=CARTESIAN_POINT('Origin',(6.00000000000001,-14.5540683672724,4.));
#3454=CARTESIAN_POINT('',(4.98850765468119,0.338808764920716,-3.));
#3455=CARTESIAN_POINT('',(6.00000000000001,-14.5540683672724,-3.));
#3456=CARTESIAN_POINT('',(4.98850765468119,0.338808764920716,-4.));
#3457=CARTESIAN_POINT('',(6.00000000000001,-14.5540683672724,-4.));
#3458=CARTESIAN_POINT('',(4.98850765468119,0.338808764920716,4.));
#3459=CARTESIAN_POINT('Origin',(0.,0.,4.));
#3460=CARTESIAN_POINT('',(-4.99999999999999,6.12323399573676E-16,-3.));
#3461=CARTESIAN_POINT('Origin',(0.,0.,-3.));
#3462=CARTESIAN_POINT('',(-4.99999999999999,6.12323399573676E-16,-4.));
#3463=CARTESIAN_POINT('Origin',(0.,0.,-4.));
#3464=CARTESIAN_POINT('',(-4.99999999999999,6.12323399573676E-16,4.));
#3465=CARTESIAN_POINT('Origin',(-4.99999999999999,-20.,4.));
#3466=CARTESIAN_POINT('',(-4.99999999999999,-19.9623339466002,3.));
#3467=CARTESIAN_POINT('',(-4.99999999999999,-19.9623339466002,-3.));
#3468=CARTESIAN_POINT('',(-4.99999999999999,-19.9623339466002,-3.));
#3469=CARTESIAN_POINT('',(-4.99999999999999,-20.,-3.));
#3470=CARTESIAN_POINT('',(-4.99999999999999,-20.,-4.));
#3471=CARTESIAN_POINT('',(-4.99999999999999,-20.,-4.));
#3472=CARTESIAN_POINT('',(-4.99999999999999,-20.,4.));
#3473=CARTESIAN_POINT('',(-4.99999999999999,-20.,4.));
#3474=CARTESIAN_POINT('',(-4.99999999999999,6.12323399573676E-16,4.));
#3475=CARTESIAN_POINT('',(-4.99999999999999,-20.,4.));
#3476=CARTESIAN_POINT('',(-4.99999999999999,6.12323399573676E-16,3.));
#3477=CARTESIAN_POINT('',(-4.99999999999999,6.12323399573676E-16,4.));
#3478=CARTESIAN_POINT('',(-4.99999999999999,-20.,3.));
#3479=CARTESIAN_POINT('Origin',(0.,-80.,4.));
#3480=CARTESIAN_POINT('',(0.,-80.,-3.));
#3481=CARTESIAN_POINT('',(0.,-80.,3.));
#3482=CARTESIAN_POINT('',(0.,-80.,4.));
#3483=CARTESIAN_POINT('',(0.,-80.,-4.));
#3484=CARTESIAN_POINT('Origin',(-103.868599666426,-35.,4.));
#3485=CARTESIAN_POINT('',(1.,-19.5540683672724,-3.));
#3486=CARTESIAN_POINT('Origin',(-103.868599666426,-35.,-3.));
#3487=CARTESIAN_POINT('',(1.,-19.5540683672724,-4.));
#3488=CARTESIAN_POINT('Origin',(-103.868599666426,-35.,-4.));
#3489=CARTESIAN_POINT('',(1.,-19.5540683672724,4.));
#3490=CARTESIAN_POINT('Origin',(1.,-19.5540683672724,4.));
#3491=CARTESIAN_POINT('',(1.,-19.5540683672724,-3.));
#3492=CARTESIAN_POINT('',(1.,-19.5540683672724,-4.));
#3493=CARTESIAN_POINT('Origin',(1.00000000000001,-14.5540683672724,4.));
#3494=CARTESIAN_POINT('',(1.00000000000001,-14.5540683672724,4.));
#3495=CARTESIAN_POINT('',(1.00000000000001,-14.5540683672724,3.));
#3496=CARTESIAN_POINT('',(1.00000000000001,-14.5540683672724,4.));
#3497=CARTESIAN_POINT('',(6.00000000000001,-14.5540683672724,3.));
#3498=CARTESIAN_POINT('',(1.00000000000001,-14.5540683672724,3.));
#3499=CARTESIAN_POINT('',(6.00000000000001,-14.5540683672724,4.));
#3500=CARTESIAN_POINT('',(6.00000000000001,-14.5540683672724,4.));
#3501=CARTESIAN_POINT('',(1.00000000000001,-14.5540683672724,4.));
#3502=CARTESIAN_POINT('Origin',(6.00000000000001,-14.5540683672724,4.));
#3503=CARTESIAN_POINT('',(4.98850765468119,0.338808764920716,3.));
#3504=CARTESIAN_POINT('',(6.00000000000001,-14.5540683672724,3.));
#3505=CARTESIAN_POINT('',(4.98850765468119,0.338808764920716,4.));
#3506=CARTESIAN_POINT('',(4.98850765468119,0.338808764920716,4.));
#3507=CARTESIAN_POINT('',(6.00000000000001,-14.5540683672724,4.));
#3508=CARTESIAN_POINT('Origin',(0.,0.,4.));
#3509=CARTESIAN_POINT('Origin',(0.,0.,3.));
#3510=CARTESIAN_POINT('Origin',(0.,0.,4.));
#3511=CARTESIAN_POINT('Origin',(-103.868599666426,-35.,4.));
#3512=CARTESIAN_POINT('Origin',(-103.868599666426,-35.,-4.));
#3513=CARTESIAN_POINT('Origin',(-103.868599666426,-35.,4.));
#3514=CARTESIAN_POINT('Origin',(-103.868599666426,-35.,4.));
#3515=CARTESIAN_POINT('',(1.,-19.5540683672724,3.));
#3516=CARTESIAN_POINT('Origin',(-103.868599666426,-35.,3.));
#3517=CARTESIAN_POINT('',(1.,-19.5540683672724,4.));
#3518=CARTESIAN_POINT('',(1.,-19.5540683672724,4.));
#3519=CARTESIAN_POINT('Origin',(-103.868599666426,-35.,4.));
#3520=CARTESIAN_POINT('Origin',(1.,-19.5540683672724,4.));
#3521=CARTESIAN_POINT('',(1.,-19.5540683672724,3.));
#3522=CARTESIAN_POINT('',(1.,-19.5540683672724,4.));
#3523=CARTESIAN_POINT('Origin',(0.,0.,4.));
#3524=CARTESIAN_POINT('Origin',(0.,0.,-4.));
#3525=CARTESIAN_POINT('Origin',(-103.868599666426,-35.,4.));
#3526=CARTESIAN_POINT('',(-4.00562885738096,-19.8875196876281,-3.));
#3527=CARTESIAN_POINT('Origin',(-103.868599666426,-35.,-3.));
#3528=CARTESIAN_POINT('',(-4.00562885738096,-19.8875196876281,3.));
#3529=CARTESIAN_POINT('',(-4.00562885738094,-19.8875196876281,4.));
#3530=CARTESIAN_POINT('Origin',(-103.868599666426,-35.,3.));
#3531=CARTESIAN_POINT('Origin',(0.,0.,3.));
#3532=CARTESIAN_POINT('Origin',(-4.49999999999999,-19.9623339466002,3.));
#3533=CARTESIAN_POINT('Origin',(0.,0.,-3.));
#3534=CARTESIAN_POINT('Origin',(-4.49999999999999,-19.9623339466002,-3.));
#3535=CARTESIAN_POINT('Origin',(-4.49999999999999,-19.9623339466002,4.));
#3536=CARTESIAN_POINT('Origin',(0.,-10.,-3.5));
#3537=CARTESIAN_POINT('Origin',(0.,-10.,3.5));
#3538=CARTESIAN_POINT('',(0.,0.,0.));
#3539=CARTESIAN_POINT('Origin',(0.,0.,-4.5));
#3540=CARTESIAN_POINT('',(-1.25,-1.53080849893419E-16,4.));
#3541=CARTESIAN_POINT('Origin',(0.,0.,4.));
#3542=CARTESIAN_POINT('',(-1.25,-1.53080849893419E-16,4.5));
#3543=CARTESIAN_POINT('',(-1.25,-1.53080849893419E-16,-4.5));
#3544=CARTESIAN_POINT('Origin',(0.,0.,4.5));
#3545=CARTESIAN_POINT('Origin',(0.,0.,-4.5));
#3546=CARTESIAN_POINT('',(-1.25,-1.53080849893419E-16,-4.5));
#3547=CARTESIAN_POINT('Origin',(0.,0.,-4.5));
#3548=CARTESIAN_POINT('',(-1.25,-1.53080849893419E-16,-4.));
#3549=CARTESIAN_POINT('',(-1.25,-1.53080849893419E-16,-4.5));
#3550=CARTESIAN_POINT('Origin',(0.,0.,-4.));
#3551=CARTESIAN_POINT('Origin',(0.,0.,5.));
#3552=CARTESIAN_POINT('',(5.3033008588991,5.30330085889912,5.));
#3553=CARTESIAN_POINT('',(-4.02974706260121,-6.32543584359663,5.));
#3554=CARTESIAN_POINT('Origin',(0.,0.,5.));
#3555=CARTESIAN_POINT('',(5.3033008588991,5.30330085889912,4.));
#3556=CARTESIAN_POINT('',(5.3033008588991,5.30330085889912,5.));
#3557=CARTESIAN_POINT('',(-4.02974706260121,-6.32543584359663,4.));
#3558=CARTESIAN_POINT('Origin',(0.,0.,4.));
#3559=CARTESIAN_POINT('',(-4.02974706260121,-6.32543584359663,5.));
#3560=CARTESIAN_POINT('Origin',(7.7979471106944,2.10154782591728,-85.1116718670025));
#3561=CARTESIAN_POINT('',(7.82039743172835,1.60205209712125,4.));
#3562=CARTESIAN_POINT('',(8.15150050128767,2.45510121651055,4.));
#3563=CARTESIAN_POINT('Origin',(7.7979471106944,2.10154782591728,4.));
#3564=CARTESIAN_POINT('',(8.15150050128767,2.45510121651055,5.));
#3565=CARTESIAN_POINT('',(8.15150050128767,2.45510121651055,-5.));
#3566=CARTESIAN_POINT('',(7.82039743172835,1.60205209712125,5.));
#3567=CARTESIAN_POINT('Origin',(7.7979471106944,2.10154782591728,5.));
#3568=CARTESIAN_POINT('',(7.82039743172835,1.60205209712125,-85.1116718670025));
#3569=CARTESIAN_POINT('Origin',(7.7979471106944,2.10154782591728,-85.1116718670025));
#3570=CARTESIAN_POINT('',(8.15150050128767,2.45510121651055,-5.));
#3571=CARTESIAN_POINT('',(7.82039743172835,1.60205209712125,-5.));
#3572=CARTESIAN_POINT('Origin',(7.7979471106944,2.10154782591728,-5.));
#3573=CARTESIAN_POINT('',(8.15150050128767,2.45510121651055,-4.));
#3574=CARTESIAN_POINT('',(8.15150050128767,2.45510121651055,-5.));
#3575=CARTESIAN_POINT('',(7.82039743172835,1.60205209712125,-4.));
#3576=CARTESIAN_POINT('Origin',(7.7979471106944,2.10154782591728,-4.));
#3577=CARTESIAN_POINT('',(7.82039743172835,1.60205209712125,-85.1116718670025));
#3578=CARTESIAN_POINT('Origin',(0.,0.,5.));
#3579=CARTESIAN_POINT('',(5.3033008588991,5.30330085889912,-4.));
#3580=CARTESIAN_POINT('',(-4.02974706260121,-6.32543584359663,-4.));
#3581=CARTESIAN_POINT('Origin',(0.,0.,-4.));
#3582=CARTESIAN_POINT('',(5.3033008588991,5.30330085889912,-5.));
#3583=CARTESIAN_POINT('',(5.3033008588991,5.30330085889912,5.));
#3584=CARTESIAN_POINT('',(-4.02974706260121,-6.32543584359663,-5.));
#3585=CARTESIAN_POINT('Origin',(0.,0.,-5.));
#3586=CARTESIAN_POINT('',(-4.02974706260121,-6.32543584359663,5.));
#3587=CARTESIAN_POINT('Origin',(17.3220165268891,-19.9280094422533,5.));
#3588=CARTESIAN_POINT('',(17.3220165268891,-19.9280094422533,-4.));
#3589=CARTESIAN_POINT('',(-4.02974706260121,-6.32543584359663,-4.));
#3590=CARTESIAN_POINT('',(17.3220165268891,-19.9280094422533,-5.));
#3591=CARTESIAN_POINT('',(17.3220165268891,-19.9280094422533,-5.));
#3592=CARTESIAN_POINT('',(17.3220165268891,-19.9280094422533,5.));
#3593=CARTESIAN_POINT('Origin',(20.3927799375376,-16.8572460316048,5.));
#3594=CARTESIAN_POINT('',(20.3927799375376,-16.8572460316048,-4.));
#3595=CARTESIAN_POINT('',(18.6250129845713,-18.6250129845711,-4.));
#3596=CARTESIAN_POINT('',(20.3927799375376,-16.8572460316048,-5.));
#3597=CARTESIAN_POINT('',(20.3927799375376,-16.8572460316048,-5.));
#3598=CARTESIAN_POINT('',(20.3927799375376,-16.8572460316048,5.));
#3599=CARTESIAN_POINT('Origin',(23.9283138434703,-20.3927799375375,5.));
#3600=CARTESIAN_POINT('',(23.9283138434703,-20.3927799375375,-4.));
#3601=CARTESIAN_POINT('',(1.76776695296638,1.76776695296638,-4.));
#3602=CARTESIAN_POINT('',(23.9283138434703,-20.3927799375375,-5.));
#3603=CARTESIAN_POINT('',(23.9283138434703,-20.3927799375375,-5.));
#3604=CARTESIAN_POINT('',(23.9283138434703,-20.3927799375375,5.));
#3605=CARTESIAN_POINT('Origin',(26.5165042944955,-30.0520382004282,5.));
#3606=CARTESIAN_POINT('',(26.5165042944955,-30.0520382004282,-4.));
#3607=CARTESIAN_POINT('',(17.2272257664368,4.61602123194541,-4.));
#3608=CARTESIAN_POINT('',(26.5165042944955,-30.0520382004282,-5.));
#3609=CARTESIAN_POINT('',(26.5165042944955,-30.0520382004282,-5.));
#3610=CARTESIAN_POINT('',(26.5165042944955,-30.0520382004282,5.));
#3611=CARTESIAN_POINT('Origin',(30.0520382004283,-26.5165042944955,5.));
#3612=CARTESIAN_POINT('',(30.0520382004283,-26.5165042944955,-4.));
#3613=CARTESIAN_POINT('',(28.2842712474616,-28.2842712474621,-4.));
#3614=CARTESIAN_POINT('',(30.0520382004283,-26.5165042944955,-5.));
#3615=CARTESIAN_POINT('',(30.0520382004283,-26.5165042944955,-5.));
#3616=CARTESIAN_POINT('',(30.0520382004283,-26.5165042944955,5.));
#3617=CARTESIAN_POINT('Origin',(37.1231060122938,-33.5875721063609,5.));
#3618=CARTESIAN_POINT('',(37.1231060122938,-33.5875721063609,-4.));
#3619=CARTESIAN_POINT('',(1.76776695296631,1.76776695296632,-4.));
#3620=CARTESIAN_POINT('',(37.1231060122938,-33.5875721063609,-5.));
#3621=CARTESIAN_POINT('',(37.1231060122938,-33.5875721063609,-5.));
#3622=CARTESIAN_POINT('',(37.1231060122938,-33.5875721063609,5.));
#3623=CARTESIAN_POINT('Origin',(40.6586399182266,-30.0520382004282,5.));
#3624=CARTESIAN_POINT('',(39.95153313704,-30.7591449816147,-4.));
#3625=CARTESIAN_POINT('',(35.3553390593274,-35.3553390593273,-4.));
#3626=CARTESIAN_POINT('',(40.6586399182266,-30.0520382004282,-5.));
#3627=CARTESIAN_POINT('',(40.6586399182266,-30.0520382004282,-5.));
#3628=CARTESIAN_POINT('',(40.6586399182266,-30.0520382004282,5.));
#3629=CARTESIAN_POINT('',(40.6586399182266,-30.0520382004282,5.));
#3630=CARTESIAN_POINT('',(37.1231060122938,-33.5875721063609,5.));
#3631=CARTESIAN_POINT('',(40.6586399182266,-30.0520382004282,5.));
#3632=CARTESIAN_POINT('',(37.1231060122938,-33.5875721063609,4.));
#3633=CARTESIAN_POINT('',(37.1231060122938,-33.5875721063609,5.));
#3634=CARTESIAN_POINT('',(39.95153313704,-30.7591449816147,4.));
#3635=CARTESIAN_POINT('',(35.3553390593274,-35.3553390593273,4.));
#3636=CARTESIAN_POINT('',(39.95153313704,-30.7591449816147,5.));
#3637=CARTESIAN_POINT('Origin',(8.,-2.39391373324695,-85.1116718670025));
#3638=CARTESIAN_POINT('',(6.96472381958992,-6.25761703840322,-4.));
#3639=CARTESIAN_POINT('Origin',(8.,-2.39391373324695,-4.));
#3640=CARTESIAN_POINT('',(6.96472381958992,-6.25761703840322,-5.));
#3641=CARTESIAN_POINT('',(6.96472381958992,-6.25761703840322,-85.1116718670025));
#3642=CARTESIAN_POINT('Origin',(8.,-2.39391373324695,-5.));
#3643=CARTESIAN_POINT('Origin',(5.3033008588991,5.30330085889912,5.));
#3644=CARTESIAN_POINT('',(5.3033008588991,5.30330085889912,5.));
#3645=CARTESIAN_POINT('',(8.15150050128767,2.45510121651055,-5.));
#3646=CARTESIAN_POINT('',(5.3033008588991,5.30330085889912,-5.));
#3647=CARTESIAN_POINT('',(5.3033008588991,5.30330085889912,5.));
#3648=CARTESIAN_POINT('Origin',(17.3220165268891,-19.9280094422533,5.));
#3649=CARTESIAN_POINT('',(17.3220165268891,-19.9280094422533,4.));
#3650=CARTESIAN_POINT('',(-4.02974706260121,-6.32543584359663,4.));
#3651=CARTESIAN_POINT('',(17.3220165268891,-19.9280094422533,5.));
#3652=CARTESIAN_POINT('',(17.3220165268891,-19.9280094422533,5.));
#3653=CARTESIAN_POINT('',(17.3220165268891,-19.9280094422533,5.));
#3654=CARTESIAN_POINT('Origin',(20.3927799375376,-16.8572460316048,5.));
#3655=CARTESIAN_POINT('',(20.3927799375376,-16.8572460316048,4.));
#3656=CARTESIAN_POINT('',(18.6250129845713,-18.6250129845711,4.));
#3657=CARTESIAN_POINT('',(20.3927799375376,-16.8572460316048,5.));
#3658=CARTESIAN_POINT('',(20.3927799375376,-16.8572460316048,5.));
#3659=CARTESIAN_POINT('',(20.3927799375376,-16.8572460316048,5.));
#3660=CARTESIAN_POINT('Origin',(23.9283138434703,-20.3927799375375,5.));
#3661=CARTESIAN_POINT('',(23.9283138434703,-20.3927799375375,4.));
#3662=CARTESIAN_POINT('',(1.76776695296638,1.76776695296638,4.));
#3663=CARTESIAN_POINT('',(23.9283138434703,-20.3927799375375,5.));
#3664=CARTESIAN_POINT('',(23.9283138434703,-20.3927799375375,5.));
#3665=CARTESIAN_POINT('',(23.9283138434703,-20.3927799375375,5.));
#3666=CARTESIAN_POINT('Origin',(26.5165042944955,-30.0520382004282,5.));
#3667=CARTESIAN_POINT('',(26.5165042944955,-30.0520382004282,4.));
#3668=CARTESIAN_POINT('',(17.2272257664368,4.61602123194541,4.));
#3669=CARTESIAN_POINT('',(26.5165042944955,-30.0520382004282,5.));
#3670=CARTESIAN_POINT('',(26.5165042944955,-30.0520382004282,5.));
#3671=CARTESIAN_POINT('',(26.5165042944955,-30.0520382004282,5.));
#3672=CARTESIAN_POINT('Origin',(30.0520382004283,-26.5165042944955,5.));
#3673=CARTESIAN_POINT('',(30.0520382004283,-26.5165042944955,4.));
#3674=CARTESIAN_POINT('',(28.2842712474616,-28.2842712474621,4.));
#3675=CARTESIAN_POINT('',(30.0520382004283,-26.5165042944955,5.));
#3676=CARTESIAN_POINT('',(30.0520382004283,-26.5165042944955,5.));
#3677=CARTESIAN_POINT('',(30.0520382004283,-26.5165042944955,5.));
#3678=CARTESIAN_POINT('Origin',(37.1231060122938,-33.5875721063609,5.));
#3679=CARTESIAN_POINT('',(1.76776695296631,1.76776695296632,4.));
#3680=CARTESIAN_POINT('',(37.1231060122938,-33.5875721063609,5.));
#3681=CARTESIAN_POINT('Origin',(5.3033008588991,5.30330085889912,5.));
#3682=CARTESIAN_POINT('',(20.4876853876369,-9.88108366983852,-5.));
#3683=CARTESIAN_POINT('',(5.3033008588991,5.30330085889912,-5.));
#3684=CARTESIAN_POINT('',(20.4876853876369,-9.88108366983852,5.));
#3685=CARTESIAN_POINT('',(20.4876853876369,-9.88108366983852,-85.1116718670025));
#3686=CARTESIAN_POINT('',(5.3033008588991,5.30330085889912,5.));
#3687=CARTESIAN_POINT('Origin',(0.,0.,5.));
#3688=CARTESIAN_POINT('',(6.96472381958992,-6.25761703840322,5.));
#3689=CARTESIAN_POINT('Origin',(8.,-2.39391373324695,5.));
#3690=CARTESIAN_POINT('',(-1.09785622885958,-4.09725522550989,5.));
#3691=CARTESIAN_POINT('Origin',(0.,0.,-5.));
#3692=CARTESIAN_POINT('',(-1.09785622885958,-4.09725522550989,-5.));
#3693=CARTESIAN_POINT('Origin',(20.4876853876369,-9.88108366983852,-85.1116718670025));
#3694=CARTESIAN_POINT('',(6.96472381958992,-6.25761703840322,4.));
#3695=CARTESIAN_POINT('',(18.5558337350586,-9.36344557963344,4.));
#3696=CARTESIAN_POINT('',(-1.09785622885958,-4.09725522550989,4.));
#3697=CARTESIAN_POINT('',(6.96472381958992,-6.25761703840322,-85.1116718670025));
#3698=CARTESIAN_POINT('',(18.5558337350586,-9.36344557963344,-4.));
#3699=CARTESIAN_POINT('',(-1.09785622885958,-4.09725522550989,-4.));
#3700=CARTESIAN_POINT('',(18.5558337350586,-9.36344557963344,-85.1116718670025));
#3701=CARTESIAN_POINT('Origin',(8.,-2.39391373324695,-85.1116718670025));
#3702=CARTESIAN_POINT('Origin',(8.,-2.39391373324695,4.));
#3703=CARTESIAN_POINT('Origin',(8.15150050128767,2.45510121651055,0.));
#3704=CARTESIAN_POINT('',(7.44439372010113,1.747994435324,4.));
#3705=CARTESIAN_POINT('',(8.15150050128767,2.45510121651055,4.));
#3706=CARTESIAN_POINT('',(7.44439372010113,1.747994435324,-4.));
#3707=CARTESIAN_POINT('',(7.44439372010113,1.747994435324,5.));
#3708=CARTESIAN_POINT('',(2.84819964238857,-2.84819964238856,-4.));
#3709=CARTESIAN_POINT('Origin',(5.3033008588991,5.30330085889912,0.));
#3710=CARTESIAN_POINT('',(4.59619407771255,4.59619407771257,-4.));
#3711=CARTESIAN_POINT('',(5.3033008588991,5.30330085889912,-4.));
#3712=CARTESIAN_POINT('',(4.59619407771255,4.59619407771257,4.));
#3713=CARTESIAN_POINT('',(4.59619407771255,4.59619407771257,0.));
#3714=CARTESIAN_POINT('',(5.3033008588991,5.30330085889912,4.));
#3715=CARTESIAN_POINT('Origin',(4.59619407771255,4.59619407771257,5.));
#3716=CARTESIAN_POINT('',(4.59619407771255,4.59619407771257,4.));
#3717=CARTESIAN_POINT('',(4.59619407771255,4.59619407771257,-4.));
#3718=CARTESIAN_POINT('Origin',(4.59619407771255,4.59619407771257,5.));
#3719=CARTESIAN_POINT('',(4.59619407771255,4.59619407771257,-4.));
#3720=CARTESIAN_POINT('',(4.59619407771255,4.59619407771257,4.));
#3721=CARTESIAN_POINT('Origin',(0.,0.,4.));
#3722=CARTESIAN_POINT('Origin',(0.,0.,-4.));
#3723=CARTESIAN_POINT('Origin',(0.,0.,-4.5));
#3724=CARTESIAN_POINT('Origin',(0.,0.,4.5));
#3725=CARTESIAN_POINT('',(0.,0.,0.));
#3726=CARTESIAN_POINT('Ctrl Pts',(18.8143835621595,-45.3725581651887,-2.29264601963605));
#3727=CARTESIAN_POINT('Ctrl Pts',(18.799421862846,-45.366692611081,-2.29601323464502));
#3728=CARTESIAN_POINT('Ctrl Pts',(18.7845100498018,-45.360314232665,-2.29875605009942));
#3729=CARTESIAN_POINT('Ctrl Pts',(18.7622518217144,-45.3499802606706,-2.30191697923756));
#3730=CARTESIAN_POINT('Ctrl Pts',(18.7548376244511,-45.3464005096126,-2.30281208768347));
#3731=CARTESIAN_POINT('Ctrl Pts',(18.7400559460073,-45.3389851193664,-2.30427767151426));
#3732=CARTESIAN_POINT('Ctrl Pts',(18.7326634287054,-45.3351353187089,-2.3048487962336));
#3733=CARTESIAN_POINT('Ctrl Pts',(18.7107560010767,-45.3232997976908,-2.30605306308975));
#3734=CARTESIAN_POINT('Ctrl Pts',(18.69647386335,-45.3150169340706,-2.30618966865469));
#3735=CARTESIAN_POINT('Ctrl Pts',(18.668502415621,-45.297660633993,-2.30516256178937));
#3736=CARTESIAN_POINT('Ctrl Pts',(18.6548195137261,-45.2885911850942,-2.3039990903213));
#3737=CARTESIAN_POINT('Ctrl Pts',(18.6280626028503,-45.269665384442,-2.3003672370976));
#3738=CARTESIAN_POINT('Ctrl Pts',(18.6150036070141,-45.2598211706463,-2.29790262175487));
#3739=CARTESIAN_POINT('Ctrl Pts',(18.5958424864585,-45.244407875027,-2.29318270097683));
#3740=CARTESIAN_POINT('Ctrl Pts',(18.5895683887268,-45.2391944776938,-2.29144761696805));
#3741=CARTESIAN_POINT('Ctrl Pts',(18.5773056208511,-45.2286717796098,-2.28767708876727));
#3742=CARTESIAN_POINT('Ctrl Pts',(18.571302721882,-45.2233510576313,-2.28563816739681));
#3743=CARTESIAN_POINT('Ctrl Pts',(18.5536922471648,-45.2072288630195,-2.27907242657322));
#3744=CARTESIAN_POINT('Ctrl Pts',(18.5424689819436,-45.1962571521417,-2.27409434987581));
#3745=CARTESIAN_POINT('Ctrl Pts',(18.5210534195265,-45.1738767847226,-2.26294902313096));
#3746=CARTESIAN_POINT('Ctrl Pts',(18.5108563517502,-45.1624608434638,-2.2567766707594));
#3747=CARTESIAN_POINT('Ctrl Pts',(18.4915255994775,-45.1392076266336,-2.24323675136636));
#3748=CARTESIAN_POINT('Ctrl Pts',(18.4823425082748,-45.1272886562345,-2.23580916151862));
#3749=CARTESIAN_POINT('Ctrl Pts',(18.4654779188592,-45.1035758058956,-2.22008460131979));
#3750=CARTESIAN_POINT('Ctrl Pts',(18.4577062314804,-45.0916806335816,-2.21173267647811));
#3751=CARTESIAN_POINT('Ctrl Pts',(18.4435024450096,-45.0678731904181,-2.19410226893954));
#3752=CARTESIAN_POINT('Ctrl Pts',(18.4370613768115,-45.0559500756431,-2.18481745164526));
#3753=CARTESIAN_POINT('Ctrl Pts',(18.4283974556018,-45.0380432871124,-2.17018589369896));
#3754=CARTESIAN_POINT('Ctrl Pts',(18.4256747602959,-45.0320672479267,-2.1651880723044));
#3755=CARTESIAN_POINT('Ctrl Pts',(18.4205692543985,-45.0201143102805,-2.15495946376726));
#3756=CARTESIAN_POINT('Ctrl Pts',(18.4181811783317,-45.0141230761169,-2.14971582230565));
#3757=CARTESIAN_POINT('Ctrl Pts',(18.411557743034,-44.996204520912,-2.13367800718911));
#3758=CARTESIAN_POINT('Ctrl Pts',(18.4079107853335,-44.9844773686462,-2.12271082270486));
#3759=CARTESIAN_POINT('Ctrl Pts',(18.4020639448891,-44.9613631523321,-2.10017046144782));
#3760=CARTESIAN_POINT('Ctrl Pts',(18.3998694271457,-44.9499903424353,-2.08860999048261));
#3761=CARTESIAN_POINT('Ctrl Pts',(18.3969224236575,-44.927612616283,-2.06491243172319));
#3762=CARTESIAN_POINT('Ctrl Pts',(18.3961709968481,-44.9166059372197,-2.05277259205872));
#3763=CARTESIAN_POINT('Ctrl Pts',(18.3961415719036,-44.9003846022915,-2.03412910558187));
#3764=CARTESIAN_POINT('Ctrl Pts',(18.3963173860228,-44.8950134660865,-2.02782648667107));
#3765=CARTESIAN_POINT('Ctrl Pts',(18.3970392739734,-44.8844199010087,-2.01513320991302));
#3766=CARTESIAN_POINT('Ctrl Pts',(18.3975826848578,-44.879219163033,-2.00876936719308));
#3767=CARTESIAN_POINT('Ctrl Pts',(18.3997509614153,-44.8639020731823,-1.98962815132851));
#3768=CARTESIAN_POINT('Ctrl Pts',(18.4019103092124,-44.8540407117655,-1.97676890218923));
#3769=CARTESIAN_POINT('Ctrl Pts',(18.407622325662,-44.835045996909,-1.95090394599962));
#3770=CARTESIAN_POINT('Ctrl Pts',(18.4111751980384,-44.825905164125,-1.93788950367134));
#3771=CARTESIAN_POINT('Ctrl Pts',(18.4196773870788,-44.8083449742005,-1.91169905664016));
#3772=CARTESIAN_POINT('Ctrl Pts',(18.4246337291704,-44.7999153918194,-1.89850633451621));
#3773=CARTESIAN_POINT('Ctrl Pts',(18.4359627695104,-44.7838395187261,-1.87201135519203));
#3774=CARTESIAN_POINT('Ctrl Pts',(18.4422430814637,-44.7763186261024,-1.85891858586588));
#3775=CARTESIAN_POINT('Ctrl Pts',(18.4560163442605,-44.7622376811399,-1.83296819839048));
#3776=CARTESIAN_POINT('Ctrl Pts',(18.4635048906187,-44.7556841943707,-1.82012124842252));
#3777=CARTESIAN_POINT('Ctrl Pts',(18.4796749688842,-44.7435444443489,-1.79468113425342));
#3778=CARTESIAN_POINT('Ctrl Pts',(18.4883628415307,-44.737956512423,-1.78208152867849));
#3779=CARTESIAN_POINT('Ctrl Pts',(18.5069294527721,-44.7277745729134,-1.75716664715693));
#3780=CARTESIAN_POINT('Ctrl Pts',(18.5168839026318,-44.7231591454028,-1.74477273547151));
#3781=CARTESIAN_POINT('Ctrl Pts',(18.5375829891438,-44.7151329976084,-1.72079652319878));
#3782=CARTESIAN_POINT('Ctrl Pts',(18.5483955659724,-44.7116778811927,-1.70911489538877));
#3783=CARTESIAN_POINT('Ctrl Pts',(18.5708927433727,-44.7058864158376,-1.68640778762084));
#3784=CARTESIAN_POINT('Ctrl Pts',(18.5825836040364,-44.703545953535,-1.67537312136182));
#3785=CARTESIAN_POINT('Ctrl Pts',(18.6068588448963,-44.6999847326678,-1.65394839029514));
#3786=CARTESIAN_POINT('Ctrl Pts',(18.619445513792,-44.6987636790236,-1.64355633794861));
#3787=CARTESIAN_POINT('Ctrl Pts',(18.645538711709,-44.6974830389479,-1.6234501769643));
#3788=CARTESIAN_POINT('Ctrl Pts',(18.6588325169338,-44.6974335055609,-1.61389957814289));
#3789=CARTESIAN_POINT('Ctrl Pts',(18.6859142215439,-44.6984777777184,-1.59576518307013));
#3790=CARTESIAN_POINT('Ctrl Pts',(18.6997000237853,-44.6995718128947,-1.58718313777874));
#3791=CARTESIAN_POINT('Ctrl Pts',(18.7277631107646,-44.7028992757828,-1.57098989163726));
#3792=CARTESIAN_POINT('Ctrl Pts',(18.7420482463831,-44.705135147643,-1.56337590956548));
#3793=CARTESIAN_POINT('Ctrl Pts',(18.7710946722565,-44.7107644468085,-1.54915862669876));
#3794=CARTESIAN_POINT('Ctrl Pts',(18.7859459094799,-44.7141859522031,-1.54252376800531));
#3795=CARTESIAN_POINT('Ctrl Pts',(18.8156397942149,-44.7221041428292,-1.53052427124137));
#3796=CARTESIAN_POINT('Ctrl Pts',(18.8305728440077,-44.7266157346991,-1.52511234349085));
#3797=CARTESIAN_POINT('Ctrl Pts',(18.860539209484,-44.7367266946174,-1.5155044665792));
#3798=CARTESIAN_POINT('Ctrl Pts',(18.8756508883745,-44.7423612795317,-1.51129385304441));
#3799=CARTESIAN_POINT('Ctrl Pts',(18.9054576403702,-44.7545267829697,-1.50424311881235));
#3800=CARTESIAN_POINT('Ctrl Pts',(18.9202547119906,-44.7610889823919,-1.50136656793277));
#3801=CARTESIAN_POINT('Ctrl Pts',(18.9495825981467,-44.7751396990536,-1.49691920365679));
#3802=CARTESIAN_POINT('Ctrl Pts',(18.9641293094195,-44.7826350228748,-1.49534501613366));
#3803=CARTESIAN_POINT('Ctrl Pts',(18.9857447788442,-44.7945759268798,-1.49397586706081));
#3804=CARTESIAN_POINT('Ctrl Pts',(18.9929278602255,-44.7986804211822,-1.49368555779672));
#3805=CARTESIAN_POINT('Ctrl Pts',(19.0072126126538,-44.8071190824507,-1.49344249033367));
#3806=CARTESIAN_POINT('Ctrl Pts',(19.0143424710875,-44.8114714840967,-1.49349117220706));
#3807=CARTESIAN_POINT('Ctrl Pts',(19.0354329844958,-44.8247714038735,-1.49415091340346));
#3808=CARTESIAN_POINT('Ctrl Pts',(19.0491062136184,-44.8339600939764,-1.49526534883766));
#3809=CARTESIAN_POINT('Ctrl Pts',(19.0757504934149,-44.8529989681212,-1.49881561860667));
#3810=CARTESIAN_POINT('Ctrl Pts',(19.0887128011736,-44.8628432034342,-1.50125064598544));
#3811=CARTESIAN_POINT('Ctrl Pts',(19.1139155845031,-44.8831828996875,-1.50744605367826));
#3812=CARTESIAN_POINT('Ctrl Pts',(19.1261415989452,-44.8936651252513,-1.51120097784455));
#3813=CARTESIAN_POINT('Ctrl Pts',(19.1439645943469,-44.9099328769387,-1.51787676636393));
#3814=CARTESIAN_POINT('Ctrl Pts',(19.1497815019618,-44.9154129298509,-1.5202634684245));
#3815=CARTESIAN_POINT('Ctrl Pts',(19.1611066834579,-44.9264248357533,-1.52532718281113));
#3816=CARTESIAN_POINT('Ctrl Pts',(19.1666295883308,-44.9319700105026,-1.52800963496645));
#3817=CARTESIAN_POINT('Ctrl Pts',(19.182766450003,-44.9487031839457,-1.53649330236943));
#3818=CARTESIAN_POINT('Ctrl Pts',(19.1929633751574,-44.9600013145975,-1.54273516166076));
#3819=CARTESIAN_POINT('Ctrl Pts',(19.2122406126713,-44.9828745059678,-1.55637255063521));
#3820=CARTESIAN_POINT('Ctrl Pts',(19.2213264422722,-44.9944588868497,-1.56377534127668));
#3821=CARTESIAN_POINT('Ctrl Pts',(19.2383462415657,-45.0178815598089,-1.5797264080401));
#3822=CARTESIAN_POINT('Ctrl Pts',(19.2463304771073,-45.0298136028999,-1.58835146880908));
#3823=CARTESIAN_POINT('Ctrl Pts',(19.2607714831931,-45.0534013484058,-1.60637132681278));
#3824=CARTESIAN_POINT('Ctrl Pts',(19.2673038350586,-45.0651515570016,-1.61582546123857));
#3825=CARTESIAN_POINT('Ctrl Pts',(19.2789889194292,-45.0885216379426,-1.63556445143045));
#3826=CARTESIAN_POINT('Ctrl Pts',(19.2841483413751,-45.1001499111597,-1.64585461771952));
#3827=CARTESIAN_POINT('Ctrl Pts',(19.2930976235061,-45.1232965562804,-1.66727425622956));
#3828=CARTESIAN_POINT('Ctrl Pts',(19.2968886296023,-45.1348186371361,-1.67840737565011));
#3829=CARTESIAN_POINT('Ctrl Pts',(19.3030533575681,-45.1577395162296,-1.70152165051547));
#3830=CARTESIAN_POINT('Ctrl Pts',(19.3053753002664,-45.1689424569227,-1.71330457990983));
#3831=CARTESIAN_POINT('Ctrl Pts',(19.3085649502556,-45.1908773666279,-1.73731958680616));
#3832=CARTESIAN_POINT('Ctrl Pts',(19.3094315307921,-45.2016060723277,-1.74954856369043));
#3833=CARTESIAN_POINT('Ctrl Pts',(19.3097256320476,-45.2225959572621,-1.77444163318775));
#3834=CARTESIAN_POINT('Ctrl Pts',(19.3091504322929,-45.2328640131764,-1.78711583153893));
#3835=CARTESIAN_POINT('Ctrl Pts',(19.3065477416738,-45.2529009468769,-1.81286399012433));
#3836=CARTESIAN_POINT('Ctrl Pts',(19.3044916971078,-45.2627436719468,-1.82604582345194));
#3837=CARTESIAN_POINT('Ctrl Pts',(19.2989881366047,-45.2815256556052,-1.8522784706461));
#3838=CARTESIAN_POINT('Ctrl Pts',(19.2955400517893,-45.290535759037,-1.86541441902233));
#3839=CARTESIAN_POINT('Ctrl Pts',(19.2872838742066,-45.3077809202632,-1.89168343393709));
#3840=CARTESIAN_POINT('Ctrl Pts',(19.2824758531213,-45.3160216986954,-1.90482330786193));
#3841=CARTESIAN_POINT('Ctrl Pts',(19.2714947564013,-45.3317383217991,-1.93111314012225));
#3842=CARTESIAN_POINT('Ctrl Pts',(19.2653276103518,-45.3392082270028,-1.94425196045163));
#3843=CARTESIAN_POINT('Ctrl Pts',(19.2515609423283,-45.3533830770125,-1.97058421507986));
#3844=CARTESIAN_POINT('Ctrl Pts',(19.244064213872,-45.3599773095852,-1.98357519226534));
#3845=CARTESIAN_POINT('Ctrl Pts',(19.2279384887284,-45.3721611568294,-2.00912118369974));
#3846=CARTESIAN_POINT('Ctrl Pts',(19.2192997653202,-45.37776054843,-2.02169452303134));
#3847=CARTESIAN_POINT('Ctrl Pts',(19.2008823814414,-45.3879779405028,-2.04643994358655));
#3848=CARTESIAN_POINT('Ctrl Pts',(19.1910930202263,-45.3925988298126,-2.05862275579914));
#3849=CARTESIAN_POINT('Ctrl Pts',(19.1703915953673,-45.4008287111318,-2.08254175691223));
#3850=CARTESIAN_POINT('Ctrl Pts',(19.1593769020686,-45.4044612308546,-2.09437589174056));
#3851=CARTESIAN_POINT('Ctrl Pts',(19.1365984286433,-45.4105559999369,-2.11715811641161));
#3852=CARTESIAN_POINT('Ctrl Pts',(19.1247946980441,-45.4130446424486,-2.12816493034605));
#3853=CARTESIAN_POINT('Ctrl Pts',(19.1003849579208,-45.4169112106896,-2.14940462118797));
#3854=CARTESIAN_POINT('Ctrl Pts',(19.0877771726989,-45.4182909661987,-2.15964088112869));
#3855=CARTESIAN_POINT('Ctrl Pts',(19.0617491248472,-45.4199293752183,-2.17933956376603));
#3856=CARTESIAN_POINT('Ctrl Pts',(19.0483317526372,-45.4201882850831,-2.1888003047611));
#3857=CARTESIAN_POINT('Ctrl Pts',(19.0206432686844,-45.4195375776723,-2.20692604496228));
#3858=CARTESIAN_POINT('Ctrl Pts',(19.0065974658149,-45.418632682757,-2.21544292771705));
#3859=CARTESIAN_POINT('Ctrl Pts',(18.9781346138199,-45.415695036091,-2.23140600796168));
#3860=CARTESIAN_POINT('Ctrl Pts',(18.9637143613756,-45.4136621054362,-2.23885416694541));
#3861=CARTESIAN_POINT('Ctrl Pts',(18.9344985968864,-45.4084658423515,-2.25268578324637));
#3862=CARTESIAN_POINT('Ctrl Pts',(18.9196997691129,-45.4053010066314,-2.25906973315595));
#3863=CARTESIAN_POINT('Ctrl Pts',(18.8972234079784,-45.399684523811,-2.26782447509019));
#3864=CARTESIAN_POINT('Ctrl Pts',(18.8896670993892,-45.3976611130282,-2.27061057640927));
#3865=CARTESIAN_POINT('Ctrl Pts',(18.8745247920546,-45.3933350465311,-2.27587916719238));
#3866=CARTESIAN_POINT('Ctrl Pts',(18.86697271241,-45.3910428501848,-2.27835075020622));
#3867=CARTESIAN_POINT('Ctrl Pts',(18.8443734352162,-45.3837824914105,-2.28528292905637));
#3868=CARTESIAN_POINT('Ctrl Pts',(18.8293452614729,-45.3784237192965,-2.28927880462709));
#3869=CARTESIAN_POINT('Ctrl Pts',(18.8143835621595,-45.3725581651887,-2.29264601963605));
#3870=CARTESIAN_POINT('Ctrl Pts',(18.6221620196843,-45.62059505756,-1.77871850124803));
#3871=CARTESIAN_POINT('Ctrl Pts',(18.6129193730699,-45.6172932558704,-1.78058192917525));
#3872=CARTESIAN_POINT('Ctrl Pts',(18.6037208544611,-45.6136589591554,-1.78208130646566));
#3873=CARTESIAN_POINT('Ctrl Pts',(18.5900102210826,-45.6077105512134,-1.78377425389336));
#3874=CARTESIAN_POINT('Ctrl Pts',(18.5854465361298,-45.6056405946596,-1.78424599704345));
#3875=CARTESIAN_POINT('Ctrl Pts',(18.576354527559,-45.6013345885701,-1.78500009038837));
#3876=CARTESIAN_POINT('Ctrl Pts',(18.5718108421278,-45.5990902159595,-1.78528264628693));
#3877=CARTESIAN_POINT('Ctrl Pts',(18.5583557915536,-45.592164749705,-1.78583455232009));
#3878=CARTESIAN_POINT('Ctrl Pts',(18.549597268328,-45.5872853986604,-1.78581522368785));
#3879=CARTESIAN_POINT('Ctrl Pts',(18.5324696592232,-45.5770009406535,-1.78502001129054));
#3880=CARTESIAN_POINT('Ctrl Pts',(18.5241044984817,-45.5715981948212,-1.7842443140869));
#3881=CARTESIAN_POINT('Ctrl Pts',(18.5077731763177,-45.560269424572,-1.78193347961354));
#3882=CARTESIAN_POINT('Ctrl Pts',(18.4998161446777,-45.554350730268,-1.78040065085215));
#3883=CARTESIAN_POINT('Ctrl Pts',(18.4881626129628,-45.5450449208074,-1.77750557246982));
#3884=CARTESIAN_POINT('Ctrl Pts',(18.4843505062967,-45.54189107573,-1.77644663525675));
#3885=CARTESIAN_POINT('Ctrl Pts',(18.4769071413954,-45.5355132808845,-1.77415492247898));
#3886=CARTESIAN_POINT('Ctrl Pts',(18.4732672288629,-45.5322824364064,-1.77292001334332));
#3887=CARTESIAN_POINT('Ctrl Pts',(18.4626004022307,-45.5224752605349,-1.7689552464585));
#3888=CARTESIAN_POINT('Ctrl Pts',(18.4558179103171,-45.5157781683263,-1.76596391369291));
#3889=CARTESIAN_POINT('Ctrl Pts',(18.4429084062604,-45.5020723540079,-1.75929249956289));
#3890=CARTESIAN_POINT('Ctrl Pts',(18.4367785698554,-45.4950591040281,-1.75560939899404));
#3891=CARTESIAN_POINT('Ctrl Pts',(18.4251947575442,-45.4807293651287,-1.74755147248085));
#3892=CARTESIAN_POINT('Ctrl Pts',(18.4197116844311,-45.4733619559223,-1.74314118482812));
#3893=CARTESIAN_POINT('Ctrl Pts',(18.4096841967476,-45.4586601759361,-1.73382309642942));
#3894=CARTESIAN_POINT('Ctrl Pts',(18.4050855722086,-45.4512635702888,-1.72888250720206));
#3895=CARTESIAN_POINT('Ctrl Pts',(18.3967294933308,-45.4364159601022,-1.71846981786302));
#3896=CARTESIAN_POINT('Ctrl Pts',(18.3929666633764,-45.4289582747971,-1.71299394688883));
#3897=CARTESIAN_POINT('Ctrl Pts',(18.387949845685,-45.4177241224448,-1.7043764995696));
#3898=CARTESIAN_POINT('Ctrl Pts',(18.3863815973451,-45.4139692966578,-1.70143483928496));
#3899=CARTESIAN_POINT('Ctrl Pts',(18.3834588294126,-45.4064475115089,-1.69541819155667));
#3900=CARTESIAN_POINT('Ctrl Pts',(18.3821013440093,-45.4026715013318,-1.69233565252243));
#3901=CARTESIAN_POINT('Ctrl Pts',(18.3783678140288,-45.3913602280059,-1.68291331926215));
#3902=CARTESIAN_POINT('Ctrl Pts',(18.3763571442371,-45.3839334687444,-1.67647740418325));
#3903=CARTESIAN_POINT('Ctrl Pts',(18.373239274455,-45.3692470015761,-1.66326464104222));
#3904=CARTESIAN_POINT('Ctrl Pts',(18.3721351020341,-45.361996292618,-1.65649525672691));
#3905=CARTESIAN_POINT('Ctrl Pts',(18.3708276406403,-45.3476781657535,-1.64263357999033));
#3906=CARTESIAN_POINT('Ctrl Pts',(18.3706250612,-45.3406095748083,-1.635539689768));
#3907=CARTESIAN_POINT('Ctrl Pts',(18.3710077529534,-45.3301503262564,-1.62465679749559));
#3908=CARTESIAN_POINT('Ctrl Pts',(18.3712517326172,-45.3266799167243,-1.62097960829253));
#3909=CARTESIAN_POINT('Ctrl Pts',(18.3719701704098,-45.3198204005466,-1.61357771003206));
#3910=CARTESIAN_POINT('Ctrl Pts',(18.3724424090973,-45.3164453844991,-1.60986862656259));
#3911=CARTESIAN_POINT('Ctrl Pts',(18.3741925883538,-45.3064826315517,-1.59871817096884));
#3912=CARTESIAN_POINT('Ctrl Pts',(18.3758024868939,-45.300037895571,-1.59123476923353));
#3913=CARTESIAN_POINT('Ctrl Pts',(18.3798873333543,-45.287560207475,-1.57619835335595));
#3914=CARTESIAN_POINT('Ctrl Pts',(18.3823625923558,-45.2815224282728,-1.56864024051346));
#3915=CARTESIAN_POINT('Ctrl Pts',(18.3881814606797,-45.2698526364099,-1.55344639789905));
#3916=CARTESIAN_POINT('Ctrl Pts',(18.3915297734654,-45.2642137421464,-1.54580098849944));
#3917=CARTESIAN_POINT('Ctrl Pts',(18.3991069351451,-45.2533791834234,-1.53046386154549));
#3918=CARTESIAN_POINT('Ctrl Pts',(18.4032741386649,-45.2482681928533,-1.52289338059093));
#3919=CARTESIAN_POINT('Ctrl Pts',(18.4123563475389,-45.2386112685697,-1.50790546647126));
#3920=CARTESIAN_POINT('Ctrl Pts',(18.4172683983267,-45.2340697519755,-1.50049420992322));
#3921=CARTESIAN_POINT('Ctrl Pts',(18.4278282750222,-45.2255558775991,-1.48583573393937));
#3922=CARTESIAN_POINT('Ctrl Pts',(18.4334801703118,-45.2215821677685,-1.47858483274337));
#3923=CARTESIAN_POINT('Ctrl Pts',(18.4455181297567,-45.2142206641317,-1.46426506544444));
#3924=CARTESIAN_POINT('Ctrl Pts',(18.4519528219293,-45.2108157610502,-1.45715123177322));
#3925=CARTESIAN_POINT('Ctrl Pts',(18.4652968721977,-45.2047449038404,-1.44340852007555));
#3926=CARTESIAN_POINT('Ctrl Pts',(18.4722504447086,-45.2020474267363,-1.43672247316454));
#3927=CARTESIAN_POINT('Ctrl Pts',(18.4866860257431,-45.1973329645429,-1.42374529115857));
#3928=CARTESIAN_POINT('Ctrl Pts',(18.4941721105413,-45.1953130577611,-1.41744886968267));
#3929=CARTESIAN_POINT('Ctrl Pts',(18.5096858061187,-45.1919542156582,-1.40524401960937));
#3930=CARTESIAN_POINT('Ctrl Pts',(18.5177148817011,-45.1906149853657,-1.39933446124003));
#3931=CARTESIAN_POINT('Ctrl Pts',(18.5343294229057,-45.1886445172451,-1.38792248147468));
#3932=CARTESIAN_POINT('Ctrl Pts',(18.542779440216,-45.188029106266,-1.38251285316967));
#3933=CARTESIAN_POINT('Ctrl Pts',(18.5599645231716,-45.1875150185148,-1.37226320603098));
#3934=CARTESIAN_POINT('Ctrl Pts',(18.5686982527055,-45.1876165784289,-1.36742418470241));
#3935=CARTESIAN_POINT('Ctrl Pts',(18.5864477638643,-45.1885360827692,-1.35831709053276));
#3936=CARTESIAN_POINT('Ctrl Pts',(18.5954684722606,-45.1893552624518,-1.35404748924571));
#3937=CARTESIAN_POINT('Ctrl Pts',(18.6137800334896,-45.1917248752601,-1.34610113724339));
#3938=CARTESIAN_POINT('Ctrl Pts',(18.6231272825575,-45.1932895780203,-1.34240702291553));
#3939=CARTESIAN_POINT('Ctrl Pts',(18.6417841046389,-45.1971209486494,-1.33575597841215));
#3940=CARTESIAN_POINT('Ctrl Pts',(18.6511507406784,-45.1993932961657,-1.33277254722322));
#3941=CARTESIAN_POINT('Ctrl Pts',(18.6699132468501,-45.204646120538,-1.32751128947911));
#3942=CARTESIAN_POINT('Ctrl Pts',(18.6793578875184,-45.207646105241,-1.32522575676464));
#3943=CARTESIAN_POINT('Ctrl Pts',(18.6979513544394,-45.214255255135,-1.32144333958208));
#3944=CARTESIAN_POINT('Ctrl Pts',(18.7071641468385,-45.2178802413143,-1.31992638960479));
#3945=CARTESIAN_POINT('Ctrl Pts',(18.7253869486455,-45.225754682879,-1.31764408095801));
#3946=CARTESIAN_POINT('Ctrl Pts',(18.7344068621661,-45.2300078746987,-1.316876927761));
#3947=CARTESIAN_POINT('Ctrl Pts',(18.7477801983432,-45.2368600692891,-1.31629654325037));
#3948=CARTESIAN_POINT('Ctrl Pts',(18.752219283311,-45.2392274939513,-1.31619867106209));
#3949=CARTESIAN_POINT('Ctrl Pts',(18.7610367701067,-45.2441187387261,-1.31619676023362));
#3950=CARTESIAN_POINT('Ctrl Pts',(18.7654325107433,-45.2466532619187,-1.3162938241929));
#3951=CARTESIAN_POINT('Ctrl Pts',(18.7784191500246,-45.2544329831877,-1.31687816890436));
#3952=CARTESIAN_POINT('Ctrl Pts',(18.7868169502624,-45.2598527540315,-1.31765275683562));
#3953=CARTESIAN_POINT('Ctrl Pts',(18.8031371766128,-45.2711680622823,-1.31995614213438));
#3954=CARTESIAN_POINT('Ctrl Pts',(18.8110542369534,-45.2770600838242,-1.3214843906258));
#3955=CARTESIAN_POINT('Ctrl Pts',(18.8264003541456,-45.2893146918086,-1.32529693961078));
#3956=CARTESIAN_POINT('Ctrl Pts',(18.8338206659933,-45.2956692062439,-1.32757795725868));
#3957=CARTESIAN_POINT('Ctrl Pts',(18.8445991939612,-45.3055898547247,-1.33159522925254));
#3958=CARTESIAN_POINT('Ctrl Pts',(18.8481102922723,-45.308941341363,-1.3330260675456));
#3959=CARTESIAN_POINT('Ctrl Pts',(18.8549328043703,-45.3156945009062,-1.33605192943852));
#3960=CARTESIAN_POINT('Ctrl Pts',(18.8582530677542,-45.3191042958294,-1.33765022769154));
#3961=CARTESIAN_POINT('Ctrl Pts',(18.867933585062,-45.3294204870494,-1.34269225948157));
#3962=CARTESIAN_POINT('Ctrl Pts',(18.8740225584048,-45.336421260905,-1.34638576214841));
#3963=CARTESIAN_POINT('Ctrl Pts',(18.8854757967299,-45.3506622005078,-1.35442702575445));
#3964=CARTESIAN_POINT('Ctrl Pts',(18.8908432353629,-45.3579082824918,-1.35877902402508));
#3965=CARTESIAN_POINT('Ctrl Pts',(18.9008330792294,-45.3726243827529,-1.36813301959756));
#3966=CARTESIAN_POINT('Ctrl Pts',(18.9054840795676,-45.380154146016,-1.37317976216689));
#3967=CARTESIAN_POINT('Ctrl Pts',(18.9138227526446,-45.3951016039498,-1.38370412631569));
#3968=CARTESIAN_POINT('Ctrl Pts',(18.9175551433971,-45.4025783442055,-1.38921665563984));
#3969=CARTESIAN_POINT('Ctrl Pts',(18.9241472981129,-45.4175069410417,-1.40071017489184));
#3970=CARTESIAN_POINT('Ctrl Pts',(18.9270110154327,-45.4249640522584,-1.40669428620247));
#3971=CARTESIAN_POINT('Ctrl Pts',(18.9318734081378,-45.4398636906155,-1.41913718051563));
#3972=CARTESIAN_POINT('Ctrl Pts',(18.9338726776514,-45.4473086206934,-1.42559807779935));
#3973=CARTESIAN_POINT('Ctrl Pts',(18.9369783416384,-45.4621742438128,-1.4390004513004));
#3974=CARTESIAN_POINT('Ctrl Pts',(18.9380587854086,-45.4694678481601,-1.44582700875946));
#3975=CARTESIAN_POINT('Ctrl Pts',(18.9393173410065,-45.4838003767252,-1.45973104908589));
#3976=CARTESIAN_POINT('Ctrl Pts',(18.9394948496878,-45.4908371992824,-1.46680673001694));
#3977=CARTESIAN_POINT('Ctrl Pts',(18.9389586363646,-45.504655487356,-1.4812020445518));
#3978=CARTESIAN_POINT('Ctrl Pts',(18.9382429617193,-45.5114415845077,-1.48852750652597));
#3979=CARTESIAN_POINT('Ctrl Pts',(18.935914549752,-45.5247359862846,-1.5034028039268));
#3980=CARTESIAN_POINT('Ctrl Pts',(18.9342813020382,-45.5312939444273,-1.51101488314489));
#3981=CARTESIAN_POINT('Ctrl Pts',(18.9301711295785,-45.543861814362,-1.52615759875804));
#3982=CARTESIAN_POINT('Ctrl Pts',(18.9276914024776,-45.5499184342165,-1.53373745384419));
#3983=CARTESIAN_POINT('Ctrl Pts',(18.9219044584414,-45.5615659591846,-1.5488905221349));
#3984=CARTESIAN_POINT('Ctrl Pts',(18.9185970863043,-45.5671606360396,-1.55646766958521));
#3985=CARTESIAN_POINT('Ctrl Pts',(18.9111518540018,-45.5778903308794,-1.5716231951062));
#3986=CARTESIAN_POINT('Ctrl Pts',(18.9070179238834,-45.5830212371186,-1.57919515593537));
#3987=CARTESIAN_POINT('Ctrl Pts',(18.8978775137544,-45.5928252580521,-1.59436601615716));
#3988=CARTESIAN_POINT('Ctrl Pts',(18.8929394538017,-45.5974219543871,-1.60184826399308));
#3989=CARTESIAN_POINT('Ctrl Pts',(18.8823875119263,-45.6059897116602,-1.61655719916668));
#3990=CARTESIAN_POINT('Ctrl Pts',(18.8767671790069,-45.6099675442075,-1.62379444292518));
#3991=CARTESIAN_POINT('Ctrl Pts',(18.8648446796018,-45.6173136869872,-1.63803320411293));
#3992=CARTESIAN_POINT('Ctrl Pts',(18.8585356910874,-45.620684256901,-1.645040886683));
#3993=CARTESIAN_POINT('Ctrl Pts',(18.8452471260023,-45.6267961002234,-1.65879399575824));
#3994=CARTESIAN_POINT('Ctrl Pts',(18.8382022586574,-45.629556299998,-1.66559567268411));
#3995=CARTESIAN_POINT('Ctrl Pts',(18.8236812226873,-45.6343318803847,-1.67868354354709));
#3996=CARTESIAN_POINT('Ctrl Pts',(18.816179049323,-45.6363659793353,-1.68500354300762));
#3997=CARTESIAN_POINT('Ctrl Pts',(18.8007069179842,-45.6397318406192,-1.69719202919393));
#3998=CARTESIAN_POINT('Ctrl Pts',(18.7927357842832,-45.6410648637206,-1.70306246701553));
#3999=CARTESIAN_POINT('Ctrl Pts',(18.7763184849427,-45.6430238072,-1.7143510708677));
#4000=CARTESIAN_POINT('Ctrl Pts',(18.7678741313109,-45.643649793127,-1.7197682782934));
#4001=CARTESIAN_POINT('Ctrl Pts',(18.750484658679,-45.6441668837513,-1.73013665595371));
#4002=CARTESIAN_POINT('Ctrl Pts',(18.7416810490484,-45.6440534227969,-1.7350030871688));
#4003=CARTESIAN_POINT('Ctrl Pts',(18.7238738472453,-45.6431037361945,-1.74411204981961));
#4004=CARTESIAN_POINT('Ctrl Pts',(18.7148682493225,-45.6422674984819,-1.74835570404536));
#4005=CARTESIAN_POINT('Ctrl Pts',(18.6966533086483,-45.6398726569234,-1.75622164832084));
#4006=CARTESIAN_POINT('Ctrl Pts',(18.6874419268025,-45.6383131841139,-1.75984420616735));
#4007=CARTESIAN_POINT('Ctrl Pts',(18.6734737700129,-45.6354195819173,-1.76479817562067));
#4008=CARTESIAN_POINT('Ctrl Pts',(18.6687815047508,-45.6343591081953,-1.76637215337371));
#4009=CARTESIAN_POINT('Ctrl Pts',(18.6593857582353,-45.6320583062489,-1.76934304099513));
#4010=CARTESIAN_POINT('Ctrl Pts',(18.6547033024031,-45.6308236309591,-1.77073381700843));
#4011=CARTESIAN_POINT('Ctrl Pts',(18.6407016991349,-45.6268695302727,-1.77462522039306));
#4012=CARTESIAN_POINT('Ctrl Pts',(18.6314046662986,-45.6238968592495,-1.77685507332082));
#4013=CARTESIAN_POINT('Ctrl Pts',(18.6221620196843,-45.62059505756,-1.77871850124803));
#4014=CARTESIAN_POINT('',(18.8905539268402,-44.7484447038542,-1.50776822046474));
#4015=CARTESIAN_POINT('',(18.8998729391632,-45.4003277760596,-2.26677057350411));
#4016=CARTESIAN_POINT('Ctrl Pts',(18.8905539268402,-44.7484447038542,-1.50776822046474));
#4017=CARTESIAN_POINT('Ctrl Pts',(18.9031610996921,-44.7535924051018,-1.50478510512969));
#4018=CARTESIAN_POINT('Ctrl Pts',(18.9153195318725,-44.7589335970676,-1.50235806754206));
#4019=CARTESIAN_POINT('Ctrl Pts',(18.9268587021024,-44.7643102161833,-1.50042690153781));
#4020=CARTESIAN_POINT('Ctrl Pts',(18.9290522874274,-44.7653323063818,-1.50005978871058));
#4021=CARTESIAN_POINT('Ctrl Pts',(18.931223536412,-44.7663556008484,-1.49971047085396));
#4022=CARTESIAN_POINT('Ctrl Pts',(18.9333713376819,-44.7673789131467,-1.49937836590513));
#4023=CARTESIAN_POINT('Ctrl Pts',(18.9338890838472,-44.767625591471,-1.49929830912049));
#4024=CARTESIAN_POINT('Ctrl Pts',(18.9344042911217,-44.7678717143732,-1.49921943230172));
#4025=CARTESIAN_POINT('Ctrl Pts',(18.9349171923153,-44.7681173760609,-1.49914167917656));
#4026=CARTESIAN_POINT('Ctrl Pts',(18.940590051698,-44.7708344767955,-1.49828170351057));
#4027=CARTESIAN_POINT('Ctrl Pts',(18.9459838062476,-44.7734936441197,-1.4975551963276));
#4028=CARTESIAN_POINT('Ctrl Pts',(18.9514090992294,-44.7762397711827,-1.49691005297651));
#4029=CARTESIAN_POINT('Ctrl Pts',(18.9567181151493,-44.7789270421458,-1.49627873659727));
#4030=CARTESIAN_POINT('Ctrl Pts',(18.9620573977875,-44.7816976275958,-1.49572532328795));
#4031=CARTESIAN_POINT('Ctrl Pts',(18.9677105039338,-44.7847152231857,-1.49524009137691));
#4032=CARTESIAN_POINT('Ctrl Pts',(18.9693228115803,-44.7855758637465,-1.49510169965027));
#4033=CARTESIAN_POINT('Ctrl Pts',(18.9709605941978,-44.7864567764315,-1.4949691090493));
#4034=CARTESIAN_POINT('Ctrl Pts',(18.9726302937406,-44.7873622109845,-1.49484274021276));
#4035=CARTESIAN_POINT('Ctrl Pts',(18.9746133338402,-44.7884375619567,-1.49469265664155));
#4036=CARTESIAN_POINT('Ctrl Pts',(18.9765824952973,-44.7895155076103,-1.4945558653122));
#4037=CARTESIAN_POINT('Ctrl Pts',(18.9785391615588,-44.7905964953401,-1.49443190148112));
#4038=CARTESIAN_POINT('Ctrl Pts',(18.9858604740922,-44.7946412571732,-1.49396806256899));
#4039=CARTESIAN_POINT('Ctrl Pts',(18.9930191605462,-44.7987358342693,-1.49368354377148));
#4040=CARTESIAN_POINT('Ctrl Pts',(19.0000696572879,-44.8029007956634,-1.49356360210869));
#4041=CARTESIAN_POINT('Ctrl Pts',(19.0072585778343,-44.8071475285728,-1.49344130560738));
#4042=CARTESIAN_POINT('Ctrl Pts',(19.0143634250414,-44.8114857800962,-1.49349151807229));
#4043=CARTESIAN_POINT('Ctrl Pts',(19.0213722794606,-44.8159054154637,-1.49371083042691));
#4044=CARTESIAN_POINT('Ctrl Pts',(19.0306063557352,-44.8217282286723,-1.49399977165603));
#4045=CARTESIAN_POINT('Ctrl Pts',(19.0396805192462,-44.8276914801336,-1.49457633549814));
#4046=CARTESIAN_POINT('Ctrl Pts',(19.0487598877559,-44.8339140289199,-1.49546367796603));
#4047=CARTESIAN_POINT('Ctrl Pts',(19.0498152273431,-44.8346373063219,-1.49556681813848));
#4048=CARTESIAN_POINT('Ctrl Pts',(19.0508706124117,-44.8353641103557,-1.49567420382705));
#4049=CARTESIAN_POINT('Ctrl Pts',(19.0519262829499,-44.8360946464113,-1.49578590842529));
#4050=CARTESIAN_POINT('Ctrl Pts',(19.0554574361024,-44.8385382446765,-1.49615955344986));
#4051=CARTESIAN_POINT('Ctrl Pts',(19.0589574262949,-44.8409997673555,-1.49657789688526));
#4052=CARTESIAN_POINT('Ctrl Pts',(19.0624281525586,-44.8434798481551,-1.49704034979883));
#4053=CARTESIAN_POINT('Ctrl Pts',(19.0758119232263,-44.8530435043288,-1.49882365486802));
#4054=CARTESIAN_POINT('Ctrl Pts',(19.0887526635036,-44.8628762409233,-1.50126029358194));
#4055=CARTESIAN_POINT('Ctrl Pts',(19.1013137349989,-44.8730137161139,-1.50434805664924));
#4056=CARTESIAN_POINT('Ctrl Pts',(19.113918973379,-44.8831868364083,-1.5074466768218));
#4057=CARTESIAN_POINT('Ctrl Pts',(19.1261274095114,-44.8936535753615,-1.51119550771856));
#4058=CARTESIAN_POINT('Ctrl Pts',(19.1380229461204,-44.9045111632162,-1.51565109795051));
#4059=CARTESIAN_POINT('Ctrl Pts',(19.143954111713,-44.9099248031066,-1.51787267435748));
#4060=CARTESIAN_POINT('Ctrl Pts',(19.1497694272033,-44.9154027344374,-1.52025795176899));
#4061=CARTESIAN_POINT('Ctrl Pts',(19.1554434156545,-44.9209197547308,-1.5227949062348));
#4062=CARTESIAN_POINT('Ctrl Pts',(19.1610906834191,-44.9264107935526,-1.52531991334367));
#4063=CARTESIAN_POINT('Ctrl Pts',(19.1666124570964,-44.9319537629785,-1.52800056793989));
#4064=CARTESIAN_POINT('Ctrl Pts',(19.1720079090184,-44.9375485200328,-1.53083713359701));
#4065=CARTESIAN_POINT('Ctrl Pts',(19.1774114710702,-44.9431516868009,-1.53367796301484));
#4066=CARTESIAN_POINT('Ctrl Pts',(19.1826920566001,-44.9488099277027,-1.53667625408543));
#4067=CARTESIAN_POINT('Ctrl Pts',(19.1878522647798,-44.9545295630061,-1.53983751083408));
#4068=CARTESIAN_POINT('Ctrl Pts',(19.1929448601249,-44.9601742554499,-1.54295734647669));
#4069=CARTESIAN_POINT('Ctrl Pts',(19.1978550853105,-44.965806463315,-1.54619576434285));
#4070=CARTESIAN_POINT('Ctrl Pts',(19.2026016057627,-44.9714383576466,-1.54955361672181));
#4071=CARTESIAN_POINT('Ctrl Pts',(19.2116168981582,-44.9821352828257,-1.55593134569646));
#4072=CARTESIAN_POINT('Ctrl Pts',(19.2200484428352,-44.9928385763987,-1.56274402992607));
#4073=CARTESIAN_POINT('Ctrl Pts',(19.227975850479,-45.0036254988957,-1.57002490172002));
#4074=CARTESIAN_POINT('Ctrl Pts',(19.2285989697718,-45.0044733850926,-1.57059720125185));
#4075=CARTESIAN_POINT('Ctrl Pts',(19.2292189565125,-45.0053217930469,-1.5711724126414));
#4076=CARTESIAN_POINT('Ctrl Pts',(19.2298358401891,-45.0061707627611,-1.57175056175926));
#4077=CARTESIAN_POINT('Ctrl Pts',(19.2375792501632,-45.0168274243037,-1.57900775759058));
#4078=CARTESIAN_POINT('Ctrl Pts',(19.244878754062,-45.0276503346359,-1.58678907892552));
#4079=CARTESIAN_POINT('Ctrl Pts',(19.2516100858949,-45.0384653157022,-1.59497152212934));
#4080=CARTESIAN_POINT('Ctrl Pts',(19.2522622252624,-45.039513083824,-1.59576424687792));
#4081=CARTESIAN_POINT('Ctrl Pts',(19.2529089949182,-45.0405607690862,-1.59656075297211));
#4082=CARTESIAN_POINT('Ctrl Pts',(19.2535502558879,-45.0416082043859,-1.59736093675765));
#4083=CARTESIAN_POINT('Ctrl Pts',(19.260249072408,-45.0525500474423,-1.60571991167469));
#4084=CARTESIAN_POINT('Ctrl Pts',(19.2664155159093,-45.0635464214966,-1.61452921889829));
#4085=CARTESIAN_POINT('Ctrl Pts',(19.2720575854048,-45.0746758327777,-1.6238743793119));
#4086=CARTESIAN_POINT('Ctrl Pts',(19.272422529821,-45.0753957134007,-1.62447884973092));
#4087=CARTESIAN_POINT('Ctrl Pts',(19.2727852644496,-45.0761161483359,-1.62508557053341));
#4088=CARTESIAN_POINT('Ctrl Pts',(19.2731457848041,-45.0768371578105,-1.62569456832308));
#4089=CARTESIAN_POINT('Ctrl Pts',(19.2746602560061,-45.0798659690052,-1.62825284167146));
#4090=CARTESIAN_POINT('Ctrl Pts',(19.2761361224734,-45.0829054847382,-1.63085164053693));
#4091=CARTESIAN_POINT('Ctrl Pts',(19.277572904716,-45.0859576117991,-1.63349352538219));
#4092=CARTESIAN_POINT('Ctrl Pts',(19.2810109144354,-45.0932609053601,-1.6398151693354));
#4093=CARTESIAN_POINT('Ctrl Pts',(19.2840733991544,-45.1003073233589,-1.64609582363185));
#4094=CARTESIAN_POINT('Ctrl Pts',(19.2868600061465,-45.1072502054313,-1.65244793958539));
#4095=CARTESIAN_POINT('Ctrl Pts',(19.2874602276128,-45.1087456681463,-1.65381615417853));
#4096=CARTESIAN_POINT('Ctrl Pts',(19.2880474864276,-45.1102363136529,-1.65518778497339));
#4097=CARTESIAN_POINT('Ctrl Pts',(19.288622513537,-45.1117236523756,-1.65656411889582));
#4098=CARTESIAN_POINT('Ctrl Pts',(19.2912948888323,-45.118635895631,-1.66296047954142));
#4099=CARTESIAN_POINT('Ctrl Pts',(19.2937068903777,-45.1254783069726,-1.66945763476478));
#4100=CARTESIAN_POINT('Ctrl Pts',(19.2959010250622,-45.1323978340472,-1.6762010109593));
#4101=CARTESIAN_POINT('Ctrl Pts',(19.2973532075745,-45.1369775056062,-1.68066409750223));
#4102=CARTESIAN_POINT('Ctrl Pts',(19.2987091190889,-45.1415908971441,-1.68523556157793));
#4103=CARTESIAN_POINT('Ctrl Pts',(19.2999702919787,-45.1462796703514,-1.68996401717864));
#4104=CARTESIAN_POINT('Ctrl Pts',(19.3003859764899,-45.147825097164,-1.69152252336869));
#4105=CARTESIAN_POINT('Ctrl Pts',(19.3007903536338,-45.1493751466532,-1.69309452547372));
#4106=CARTESIAN_POINT('Ctrl Pts',(19.3011833659943,-45.1509312276157,-1.69468174294826));
#4107=CARTESIAN_POINT('Ctrl Pts',(19.3028171351878,-45.1573999227367,-1.70127987388149));
#4108=CARTESIAN_POINT('Ctrl Pts',(19.3041469608748,-45.1635341686414,-1.70769026657886));
#4109=CARTESIAN_POINT('Ctrl Pts',(19.3052506878946,-45.1695067470371,-1.71406487112993));
#4110=CARTESIAN_POINT('Ctrl Pts',(19.3058999584912,-45.173020133471,-1.717814750607));
#4111=CARTESIAN_POINT('Ctrl Pts',(19.3064700252133,-45.176477240148,-1.72155252468992));
#4112=CARTESIAN_POINT('Ctrl Pts',(19.3069691692539,-45.1799106820285,-1.7253113759015));
#4113=CARTESIAN_POINT('Ctrl Pts',(19.3078288407013,-45.1858240691695,-1.73178521270814));
#4114=CARTESIAN_POINT('Ctrl Pts',(19.3084803198211,-45.1916671269783,-1.73831990863014));
#4115=CARTESIAN_POINT('Ctrl Pts',(19.3089258684228,-45.1975919843597,-1.74509559154831));
#4116=CARTESIAN_POINT('Ctrl Pts',(19.3092823464461,-45.2023323907711,-1.75051673313525));
#4117=CARTESIAN_POINT('Ctrl Pts',(19.3095062324181,-45.2071249057774,-1.75609237576449));
#4118=CARTESIAN_POINT('Ctrl Pts',(19.3095767014592,-45.2120403257133,-1.76192141946182));
#4119=CARTESIAN_POINT('Ctrl Pts',(19.3095769951772,-45.2120608133933,-1.76194571516467));
#4120=CARTESIAN_POINT('Ctrl Pts',(19.3095772861822,-45.2120813019672,-1.7619700138185));
#4121=CARTESIAN_POINT('Ctrl Pts',(19.3095775744728,-45.2121017914341,-1.76199431542308));
#4122=CARTESIAN_POINT('Ctrl Pts',(19.3096500706704,-45.2172542611667,-1.76810542035325));
#4123=CARTESIAN_POINT('Ctrl Pts',(19.3095501662677,-45.2224648859554,-1.77440566660266));
#4124=CARTESIAN_POINT('Ctrl Pts',(19.3092543196308,-45.2277160746578,-1.7808883526774));
#4125=CARTESIAN_POINT('Ctrl Pts',(19.3091160779735,-45.2301698224415,-1.78391754806325));
#4126=CARTESIAN_POINT('Ctrl Pts',(19.3089694464571,-45.2321010041524,-1.78632752666564));
#4127=CARTESIAN_POINT('Ctrl Pts',(19.3088187707449,-45.2338621207923,-1.78853667120843));
#4128=CARTESIAN_POINT('Ctrl Pts',(19.3086457077997,-45.2358849022229,-1.79107404803929));
#4129=CARTESIAN_POINT('Ctrl Pts',(19.3084671105678,-45.2376833156781,-1.79334660829998));
#4130=CARTESIAN_POINT('Ctrl Pts',(19.3082279498134,-45.2397710718633,-1.79600629485637));
#4131=CARTESIAN_POINT('Ctrl Pts',(19.3081111756757,-45.240790452861,-1.79730493018301));
#4132=CARTESIAN_POINT('Ctrl Pts',(19.3079846031041,-45.2418281112385,-1.79863218212924));
#4133=CARTESIAN_POINT('Ctrl Pts',(19.3078472833032,-45.2428838188181,-1.79998843184757));
#4134=CARTESIAN_POINT('Ctrl Pts',(19.3072761515731,-45.2472746502375,-1.80562925890165));
#4135=CARTESIAN_POINT('Ctrl Pts',(19.306514269498,-45.2519944004966,-1.81179500409166));
#4136=CARTESIAN_POINT('Ctrl Pts',(19.3054899970412,-45.2569968413792,-1.81847964198376));
#4137=CARTESIAN_POINT('Ctrl Pts',(19.3048735218124,-45.2600076427211,-1.82250290127023));
#4138=CARTESIAN_POINT('Ctrl Pts',(19.3041618274159,-45.2631203030561,-1.82671358764469));
#4139=CARTESIAN_POINT('Ctrl Pts',(19.3033379472344,-45.2663183805069,-1.83110364640795));
#4140=CARTESIAN_POINT('Ctrl Pts',(19.3028516227151,-45.2682061592321,-1.83369503441009));
#4141=CARTESIAN_POINT('Ctrl Pts',(19.3023186401626,-45.2701521550093,-1.83638798495598));
#4142=CARTESIAN_POINT('Ctrl Pts',(19.3017373109881,-45.272136535723,-1.83915988629776));
#4143=CARTESIAN_POINT('Ctrl Pts',(19.3004282344149,-45.2766050991776,-1.8454018422643));
#4144=CARTESIAN_POINT('Ctrl Pts',(19.2988710018605,-45.2812824487729,-1.85206311467574));
#4145=CARTESIAN_POINT('Ctrl Pts',(19.2970708305084,-45.2859874631502,-1.85892298274384));
#4146=CARTESIAN_POINT('Ctrl Pts',(19.2955249874694,-45.290027752823,-1.86481368825293));
#4147=CARTESIAN_POINT('Ctrl Pts',(19.2938005148776,-45.2940886659696,-1.87085074760323));
#4148=CARTESIAN_POINT('Ctrl Pts',(19.2919279277246,-45.2980702360208,-1.87689341384836));
#4149=CARTESIAN_POINT('Ctrl Pts',(19.291756070827,-45.2984356450622,-1.87744798022584));
#4150=CARTESIAN_POINT('Ctrl Pts',(19.2915838951129,-45.2987984610612,-1.87799965670778));
#4151=CARTESIAN_POINT('Ctrl Pts',(19.2914114387417,-45.2991587065637,-1.87854844423543));
#4152=CARTESIAN_POINT('Ctrl Pts',(19.2882717859622,-45.30571715254,-1.88853939020666));
#4153=CARTESIAN_POINT('Ctrl Pts',(19.2850429685109,-45.3114291131316,-1.89757671877641));
#4154=CARTESIAN_POINT('Ctrl Pts',(19.2819223052065,-45.316417591916,-1.90567353726888));
#4155=CARTESIAN_POINT('Ctrl Pts',(19.2802373747464,-45.3191110064351,-1.91004522840538));
#4156=CARTESIAN_POINT('Ctrl Pts',(19.2785831810204,-45.3215930602608,-1.91414275007192));
#4157=CARTESIAN_POINT('Ctrl Pts',(19.2769853047611,-45.3238800102474,-1.91796822399195));
#4158=CARTESIAN_POINT('Ctrl Pts',(19.276955266244,-45.3239230026794,-1.91804013917522));
#4159=CARTESIAN_POINT('Ctrl Pts',(19.2769252476959,-45.3239659259204,-1.91811195788365));
#4160=CARTESIAN_POINT('Ctrl Pts',(19.2768952492667,-45.3240087800738,-1.91818368013959));
#4161=CARTESIAN_POINT('Ctrl Pts',(19.2745234678546,-45.3273969802972,-1.9238542941712));
#4162=CARTESIAN_POINT('Ctrl Pts',(19.272276852796,-45.3303569483095,-1.92892674082638));
#4163=CARTESIAN_POINT('Ctrl Pts',(19.2702183165253,-45.3329374402795,-1.93341671392623));
#4164=CARTESIAN_POINT('Ctrl Pts',(19.26918904839,-45.3342276862644,-1.93566170047616));
#4165=CARTESIAN_POINT('Ctrl Pts',(19.2682683746316,-45.3353511621537,-1.9376329604304));
#4166=CARTESIAN_POINT('Ctrl Pts',(19.2671920722735,-45.3366292732086,-1.93989520389112));
#4167=CARTESIAN_POINT('Ctrl Pts',(19.2662154445237,-45.3377890204804,-1.94194794466969));
#4168=CARTESIAN_POINT('Ctrl Pts',(19.2651113457867,-45.3390764142967,-1.94424020849365));
#4169=CARTESIAN_POINT('Ctrl Pts',(19.2636480525984,-45.3407128473262,-1.94719472898812));
#4170=CARTESIAN_POINT('Ctrl Pts',(19.2634987089253,-45.3408798616479,-1.94749626728975));
#4171=CARTESIAN_POINT('Ctrl Pts',(19.2633455833603,-45.341050489925,-1.94780470520987));
#4172=CARTESIAN_POINT('Ctrl Pts',(19.2631883989319,-45.3412249511355,-1.94812049329096));
#4173=CARTESIAN_POINT('Ctrl Pts',(19.2616260730571,-45.3429589986225,-1.95125925133951));
#4174=CARTESIAN_POINT('Ctrl Pts',(19.260044246205,-45.3446482119081,-1.95435747676277));
#4175=CARTESIAN_POINT('Ctrl Pts',(19.2584442081375,-45.3462956982991,-1.95741801675829));
#4176=CARTESIAN_POINT('Ctrl Pts',(19.2530911545275,-45.3518074940197,-1.96765729481361));
#4177=CARTESIAN_POINT('Ctrl Pts',(19.2475997168375,-45.356787186144,-1.9773523720224));
#4178=CARTESIAN_POINT('Ctrl Pts',(19.2420166250089,-45.3613450400677,-1.98660396903331));
#4179=CARTESIAN_POINT('Ctrl Pts',(19.2400197366427,-45.3629752345467,-1.98991296107686));
#4180=CARTESIAN_POINT('Ctrl Pts',(19.2380131049024,-45.3645492458353,-1.9931612156242));
#4181=CARTESIAN_POINT('Ctrl Pts',(19.2360013513002,-45.3660692332073,-1.99634818798254));
#4182=CARTESIAN_POINT('Ctrl Pts',(19.2343601682657,-45.3673092347089,-1.99894811123359));
#4183=CARTESIAN_POINT('Ctrl Pts',(19.2327151668666,-45.3685136887886,-2.00150801558279));
#4184=CARTESIAN_POINT('Ctrl Pts',(19.2310684958453,-45.3696838352387,-2.00402793563221));
#4185=CARTESIAN_POINT('Ctrl Pts',(19.2291441073201,-45.3710513314613,-2.00697285004734));
#4186=CARTESIAN_POINT('Ctrl Pts',(19.227397030422,-45.3722491451667,-2.00959402269974));
#4187=CARTESIAN_POINT('Ctrl Pts',(19.2255353703308,-45.3734861835637,-2.01233998107606));
#4188=CARTESIAN_POINT('Ctrl Pts',(19.2238513499697,-45.3746051836745,-2.01482391992113));
#4189=CARTESIAN_POINT('Ctrl Pts',(19.2220734552544,-45.3757561868767,-2.01740993160128));
#4190=CARTESIAN_POINT('Ctrl Pts',(19.2199591852644,-45.3770711300371,-2.02042077054629));
#4191=CARTESIAN_POINT('Ctrl Pts',(19.2167080362679,-45.379093140545,-2.02505058890496));
#4192=CARTESIAN_POINT('Ctrl Pts',(19.213416289607,-45.3810245230521,-2.02959939975511));
#4193=CARTESIAN_POINT('Ctrl Pts',(19.2100910410519,-45.3828692664555,-2.03406719489437));
#4194=CARTESIAN_POINT('Ctrl Pts',(19.2043102415861,-45.3860762723393,-2.04183426172472));
#4195=CARTESIAN_POINT('Ctrl Pts',(19.198424016323,-45.3890224338998,-2.0493605201506));
#4196=CARTESIAN_POINT('Ctrl Pts',(19.192473591163,-45.3917248373075,-2.05663869990211));
#4197=CARTESIAN_POINT('Ctrl Pts',(19.1886352797465,-45.3934680179328,-2.06133347711209));
#4198=CARTESIAN_POINT('Ctrl Pts',(19.1847250305082,-45.3951304340046,-2.06598050218204));
#4199=CARTESIAN_POINT('Ctrl Pts',(19.1807423013201,-45.3967137749435,-2.07058224811008));
#4200=CARTESIAN_POINT('Ctrl Pts',(19.1703387758504,-45.4008497146488,-2.08260274428377));
#4201=CARTESIAN_POINT('Ctrl Pts',(19.159340113541,-45.4044710910164,-2.09441259586237));
#4202=CARTESIAN_POINT('Ctrl Pts',(19.1479876051885,-45.4075086579881,-2.10576692178429));
#4203=CARTESIAN_POINT('Ctrl Pts',(19.1366043896562,-45.4105544412158,-2.11715195980231));
#4204=CARTESIAN_POINT('Ctrl Pts',(19.1248241373798,-45.4130400365554,-2.12813908010357));
#4205=CARTESIAN_POINT('Ctrl Pts',(19.1125897171975,-45.4149780078223,-2.13878461269783));
#4206=CARTESIAN_POINT('Ctrl Pts',(19.1004590408702,-45.4168995457309,-2.14933987468066));
#4207=CARTESIAN_POINT('Ctrl Pts',(19.0878801520033,-45.4182845655764,-2.15956267184218));
#4208=CARTESIAN_POINT('Ctrl Pts',(19.0747630524034,-45.4191102447313,-2.16949006944939));
#4209=CARTESIAN_POINT('Ctrl Pts',(19.0700168171052,-45.4194090049503,-2.1730821566013));
#4210=CARTESIAN_POINT('Ctrl Pts',(19.0652003300979,-45.4196343284435,-2.17663517975666));
#4211=CARTESIAN_POINT('Ctrl Pts',(19.060307729625,-45.4197834514901,-2.18015001824002));
#4212=CARTESIAN_POINT('Ctrl Pts',(19.0517437089387,-45.4200444768615,-2.18630240073015));
#4213=CARTESIAN_POINT('Ctrl Pts',(19.0431772022301,-45.4200671915454,-2.19217450958827));
#4214=CARTESIAN_POINT('Ctrl Pts',(19.0344874410032,-45.419862988065,-2.19786305520717));
#4215=CARTESIAN_POINT('Ctrl Pts',(19.0250894389292,-45.4196421414063,-2.20401523386074));
#4216=CARTESIAN_POINT('Ctrl Pts',(19.0156502563949,-45.4191585088715,-2.20988554243695));
#4217=CARTESIAN_POINT('Ctrl Pts',(19.006007375568,-45.4184031647075,-2.21557544213857));
#4218=CARTESIAN_POINT('Ctrl Pts',(19.0015104970313,-45.4180509161399,-2.21822888028673));
#4219=CARTESIAN_POINT('Ctrl Pts',(18.9969691419846,-45.4176390560957,-2.22084259167287));
#4220=CARTESIAN_POINT('Ctrl Pts',(18.9923659355898,-45.4171639503319,-2.22342427356174));
#4221=CARTESIAN_POINT('Ctrl Pts',(18.9888660975559,-45.4168027253336,-2.22538713763762));
#4222=CARTESIAN_POINT('Ctrl Pts',(18.9853303025957,-45.4164048969542,-2.22733157337029));
#4223=CARTESIAN_POINT('Ctrl Pts',(18.9817504658063,-45.4159679276941,-2.22926016950443));
#4224=CARTESIAN_POINT('Ctrl Pts',(18.9708305376768,-45.414634997397,-2.23514315591277));
#4225=CARTESIAN_POINT('Ctrl Pts',(18.9599302006986,-45.4129890646533,-2.24064569461223));
#4226=CARTESIAN_POINT('Ctrl Pts',(18.9491064785268,-45.411063974465,-2.24576997387064));
#4227=CARTESIAN_POINT('Ctrl Pts',(18.9461921080148,-45.4105456291131,-2.24714972550591));
#4228=CARTESIAN_POINT('Ctrl Pts',(18.9432831789363,-45.4100070429297,-2.24850212658035));
#4229=CARTESIAN_POINT('Ctrl Pts',(18.9403808821526,-45.4094489146347,-2.24982720828383));
#4230=CARTESIAN_POINT('Ctrl Pts',(18.9335402930706,-45.4081334301734,-2.25295036904543));
#4231=CARTESIAN_POINT('Ctrl Pts',(18.9267361216311,-45.4067092269099,-2.25592187358363));
#4232=CARTESIAN_POINT('Ctrl Pts',(18.919980869073,-45.4051857902904,-2.25874456724948));
#4233=CARTESIAN_POINT('Ctrl Pts',(18.9164979549471,-45.4044003275891,-2.26019990878666));
#4234=CARTESIAN_POINT('Ctrl Pts',(18.9133662240863,-45.4036676302014,-2.2614777053349));
#4235=CARTESIAN_POINT('Ctrl Pts',(18.9100657264646,-45.4028709291528,-2.26279585730047));
#4236=CARTESIAN_POINT('Ctrl Pts',(18.908352626479,-45.402457407099,-2.26348003477071));
#4237=CARTESIAN_POINT('Ctrl Pts',(18.9065938749453,-45.4020260756094,-2.26417455035125));
#4238=CARTESIAN_POINT('Ctrl Pts',(18.9047155105794,-45.4015567031749,-2.26490618841246));
#4239=CARTESIAN_POINT('Ctrl Pts',(18.9031937725225,-45.4011764458034,-2.26549891765171));
#4240=CARTESIAN_POINT('Ctrl Pts',(18.901592767696,-45.4007709222593,-2.26611618194192));
#4241=CARTESIAN_POINT('Ctrl Pts',(18.8998729343624,-45.4003278468303,-2.26677060880248));
#4242=CARTESIAN_POINT('',(18.688654621475,-45.2109506804125,-1.32333454805209));
#4243=CARTESIAN_POINT('',(18.8905539268375,-44.7484447038531,-1.50776822046538));
#4244=CARTESIAN_POINT('',(18.6221620191364,-45.6205950568764,-1.77871850220987));
#4245=CARTESIAN_POINT('Ctrl Pts',(18.6221620189044,-45.6205950572814,-1.77871850140526));
#4246=CARTESIAN_POINT('Ctrl Pts',(18.6581806165478,-45.633462179895,-1.77145672208729));
#4247=CARTESIAN_POINT('Ctrl Pts',(18.6945296453429,-45.6411632239077,-1.75873958924297));
#4248=CARTESIAN_POINT('Ctrl Pts',(18.7659446834003,-45.6457061633278,-1.72295727333315));
#4249=CARTESIAN_POINT('Ctrl Pts',(18.8000184558857,-45.6419289228715,-1.69982222343669));
#4250=CARTESIAN_POINT('Ctrl Pts',(18.8596085346286,-45.6226944096372,-1.64648369257765));
#4251=CARTESIAN_POINT('Ctrl Pts',(18.8843459826501,-45.6074811389323,-1.61696981583715));
#4252=CARTESIAN_POINT('Ctrl Pts',(18.9243319236507,-45.5642815965227,-1.55028617227719));
#4253=CARTESIAN_POINT('Ctrl Pts',(18.9334400302693,-45.5387736862257,-1.51911880037033));
#4254=CARTESIAN_POINT('Ctrl Pts',(18.9407266713295,-45.4973521054937,-1.47275350501765));
#4255=CARTESIAN_POINT('Ctrl Pts',(18.9410687526231,-45.4684948170116,-1.44313131313073));
#4256=CARTESIAN_POINT('Ctrl Pts',(18.9201436069681,-45.4035479484512,-1.38874059277084));
#4257=CARTESIAN_POINT('Ctrl Pts',(18.9036875951198,-45.3736809974723,-1.367595125502));
#4258=CARTESIAN_POINT('Ctrl Pts',(18.8591032411742,-45.3175272792895,-1.33556085947497));
#4259=CARTESIAN_POINT('Ctrl Pts',(18.8317143369514,-45.2917456840402,-1.32476877134019));
#4260=CARTESIAN_POINT('Ctrl Pts',(18.7832988662914,-45.2570891704194,-1.31682541411965));
#4261=CARTESIAN_POINT('Ctrl Pts',(18.7651342495118,-45.2459423680159,-1.31573764809258));
#4262=CARTESIAN_POINT('Ctrl Pts',(18.7275364667659,-45.2263255413164,-1.31700978595565));
#4263=CARTESIAN_POINT('Ctrl Pts',(18.7080536577264,-45.2178461743263,-1.31938825619245));
#4264=CARTESIAN_POINT('Ctrl Pts',(18.6886546214932,-45.2109506803708,-1.32333454806873));
#4265=CARTESIAN_POINT('',(18.814383572052,-45.3725581690366,-2.29264601746227));
#4266=CARTESIAN_POINT('',(18.8143835735432,-45.3725581696516,-2.29264601707409));
#4267=CARTESIAN_POINT('Origin',(18.8502672096237,-45.0583616020844,-1.90494085304907));
#4268=CARTESIAN_POINT('Ctrl Pts',(3.62216201968442,-19.8058202438613,-1.94799199564959));
#4269=CARTESIAN_POINT('Ctrl Pts',(3.34425572651223,-20.2137053466864,-1.54490813204841));
#4270=CARTESIAN_POINT('Ctrl Pts',(3.25594179788809,-20.5121292468035,-0.988830267143717));
#4271=CARTESIAN_POINT('Ctrl Pts',(3.16762786926396,-20.8105531469205,-0.432752402239027));
#4272=CARTESIAN_POINT('Ctrl Pts',(3.3076189187292,-20.9771651064803,0.166181422977342));
#4273=CARTESIAN_POINT('Ctrl Pts',(3.44760996819445,-21.1437770660401,0.765115248193711));
#4274=CARTESIAN_POINT('Ctrl Pts',(3.80940000840298,-21.1823333185883,1.28827884419634));
#4275=CARTESIAN_POINT('Ctrl Pts',(4.17119004861151,-21.2208895711365,1.81144244019896));
#4276=CARTESIAN_POINT('Ctrl Pts',(4.70434308191443,-21.1605093534924,2.15521684061908));
#4277=CARTESIAN_POINT('Ctrl Pts',(5.23749611521735,-21.1001291358485,2.49899124103919));
#4278=CARTESIAN_POINT('Ctrl Pts',(5.8576356015542,-20.9895272661294,2.59528770975726));
#4279=CARTESIAN_POINT('Ctrl Pts',(6.47777508789106,-20.8789253964104,2.69158417847533));
#4280=CARTESIAN_POINT('Ctrl Pts',(7.08329575335921,-20.7767637068552,2.52133001886304));
#4281=CARTESIAN_POINT('Ctrl Pts',(7.68881641882736,-20.6746020173,2.35107585925076));
#4282=CARTESIAN_POINT('Ctrl Pts',(8.18100842628526,-20.6378706589539,1.94799199564959));
#4283=CARTESIAN_POINT('Ctrl Pts',(8.67320043374317,-20.6011393006078,1.54490813204841));
#4284=CARTESIAN_POINT('Ctrl Pts',(8.97580007665302,-20.6738691449698,0.988830267143717));
#4285=CARTESIAN_POINT('Ctrl Pts',(9.27839971956287,-20.7465989893318,0.432752402239027));
#4286=CARTESIAN_POINT('Ctrl Pts',(9.35269438438334,-20.9511407742511,-0.166181422977342));
#4287=CARTESIAN_POINT('Ctrl Pts',(9.4269890492038,-21.1556825591703,-0.765115248193711));
#4288=CARTESIAN_POINT('Ctrl Pts',(9.27948472328098,-21.4882800511012,-1.28827884419634));
#4289=CARTESIAN_POINT('Ctrl Pts',(9.13198039735816,-21.8208775430321,-1.81144244019896));
#4290=CARTESIAN_POINT('Ctrl Pts',(8.81311307834095,-22.2524115051551,-2.15521684061908));
#4291=CARTESIAN_POINT('Ctrl Pts',(8.49424575932375,-22.6839454672782,-2.49899124103919));
#4292=CARTESIAN_POINT('Ctrl Pts',(8.0883919872726,-23.1657010814762,-2.59528770975726));
#4293=CARTESIAN_POINT('Ctrl Pts',(7.68253821522146,-23.6474566956743,-2.69158417847533));
#4294=CARTESIAN_POINT('Ctrl Pts',(7.29130326403902,-24.1207721297085,-2.52133001886305));
#4295=CARTESIAN_POINT('Ctrl Pts',(6.90006831285659,-24.5940875637428,-2.35107585925076));
#4296=CARTESIAN_POINT('Ctrl Pts',(6.62216201968439,-25.0019726665679,-1.94799199564959));
#4297=CARTESIAN_POINT('Ctrl Pts',(6.34425572651219,-25.4098577693931,-1.54490813204841));
#4298=CARTESIAN_POINT('Ctrl Pts',(6.25594179788806,-25.7082816695101,-0.988830267143717));
#4299=CARTESIAN_POINT('Ctrl Pts',(6.16762786926392,-26.0067055696272,-0.432752402239027));
#4300=CARTESIAN_POINT('Ctrl Pts',(6.30761891872917,-26.1733175291869,0.166181422977342));
#4301=CARTESIAN_POINT('Ctrl Pts',(6.44760996819441,-26.3399294887468,0.765115248193711));
#4302=CARTESIAN_POINT('Ctrl Pts',(6.80940000840295,-26.3784857412949,1.28827884419634));
#4303=CARTESIAN_POINT('Ctrl Pts',(7.17119004861148,-26.4170419938431,1.81144244019896));
#4304=CARTESIAN_POINT('Ctrl Pts',(7.7043430819144,-26.3566617761991,2.15521684061908));
#4305=CARTESIAN_POINT('Ctrl Pts',(8.23749611521731,-26.2962815585551,2.49899124103919));
#4306=CARTESIAN_POINT('Ctrl Pts',(8.85763560155417,-26.1856796888361,2.59528770975726));
#4307=CARTESIAN_POINT('Ctrl Pts',(9.47777508789103,-26.0750778191171,2.69158417847533));
#4308=CARTESIAN_POINT('Ctrl Pts',(10.0832957533592,-25.9729161295619,2.52133001886304));
#4309=CARTESIAN_POINT('Ctrl Pts',(10.6888164188273,-25.8707544400067,2.35107585925076));
#4310=CARTESIAN_POINT('Ctrl Pts',(11.1810084262852,-25.8340230816606,1.94799199564959));
#4311=CARTESIAN_POINT('Ctrl Pts',(11.6732004337431,-25.7972917233145,1.54490813204841));
#4312=CARTESIAN_POINT('Ctrl Pts',(11.975800076653,-25.8700215676765,0.988830267143717));
#4313=CARTESIAN_POINT('Ctrl Pts',(12.2783997195628,-25.9427514120385,0.432752402239027));
#4314=CARTESIAN_POINT('Ctrl Pts',(12.3526943843833,-26.1472931969577,-0.166181422977342));
#4315=CARTESIAN_POINT('Ctrl Pts',(12.4269890492038,-26.351834981877,-0.765115248193711));
#4316=CARTESIAN_POINT('Ctrl Pts',(12.279484723281,-26.6844324738078,-1.28827884419634));
#4317=CARTESIAN_POINT('Ctrl Pts',(12.1319803973581,-27.0170299657387,-1.81144244019896));
#4318=CARTESIAN_POINT('Ctrl Pts',(11.8131130783409,-27.4485639278618,-2.15521684061908));
#4319=CARTESIAN_POINT('Ctrl Pts',(11.4942457593237,-27.8800978899848,-2.49899124103919));
#4320=CARTESIAN_POINT('Ctrl Pts',(11.0883919872726,-28.3618535041829,-2.59528770975726));
#4321=CARTESIAN_POINT('Ctrl Pts',(10.6825382152214,-28.8436091183809,-2.69158417847533));
#4322=CARTESIAN_POINT('Ctrl Pts',(10.291303264039,-29.3169245524152,-2.52133001886305));
#4323=CARTESIAN_POINT('Ctrl Pts',(9.90006831285655,-29.7902399864494,-2.35107585925076));
#4324=CARTESIAN_POINT('Ctrl Pts',(9.62216201968436,-30.1981250892746,-1.94799199564959));
#4325=CARTESIAN_POINT('Ctrl Pts',(9.34425572651217,-30.6060101920997,-1.54490813204841));
#4326=CARTESIAN_POINT('Ctrl Pts',(9.25594179788803,-30.9044340922168,-0.988830267143717));
#4327=CARTESIAN_POINT('Ctrl Pts',(9.16762786926389,-31.2028579923338,-0.432752402239027));
#4328=CARTESIAN_POINT('Ctrl Pts',(9.30761891872914,-31.3694699518936,0.166181422977342));
#4329=CARTESIAN_POINT('Ctrl Pts',(9.44760996819438,-31.5360819114534,0.765115248193711));
#4330=CARTESIAN_POINT('Ctrl Pts',(9.80940000840292,-31.5746381640016,1.28827884419634));
#4331=CARTESIAN_POINT('Ctrl Pts',(10.1711900486115,-31.6131944165497,1.81144244019896));
#4332=CARTESIAN_POINT('Ctrl Pts',(10.7043430819144,-31.5528141989058,2.15521684061908));
#4333=CARTESIAN_POINT('Ctrl Pts',(11.2374961152173,-31.4924339812617,2.49899124103919));
#4334=CARTESIAN_POINT('Ctrl Pts',(11.8576356015541,-31.3818321115427,2.59528770975726));
#4335=CARTESIAN_POINT('Ctrl Pts',(12.477775087891,-31.2712302418237,2.69158417847533));
#4336=CARTESIAN_POINT('Ctrl Pts',(13.0832957533591,-31.1690685522685,2.52133001886304));
#4337=CARTESIAN_POINT('Ctrl Pts',(13.6888164188273,-31.0669068627133,2.35107585925076));
#4338=CARTESIAN_POINT('Ctrl Pts',(14.1810084262852,-31.0301755043672,1.94799199564959));
#4339=CARTESIAN_POINT('Ctrl Pts',(14.6732004337431,-30.9934441460211,1.54490813204841));
#4340=CARTESIAN_POINT('Ctrl Pts',(14.975800076653,-31.0661739903831,0.988830267143717));
#4341=CARTESIAN_POINT('Ctrl Pts',(15.2783997195628,-31.1389038347451,0.432752402239027));
#4342=CARTESIAN_POINT('Ctrl Pts',(15.3526943843833,-31.3434456196644,-0.166181422977342));
#4343=CARTESIAN_POINT('Ctrl Pts',(15.4269890492037,-31.5479874045836,-0.765115248193711));
#4344=CARTESIAN_POINT('Ctrl Pts',(15.2794847232809,-31.8805848965145,-1.28827884419634));
#4345=CARTESIAN_POINT('Ctrl Pts',(15.1319803973581,-32.2131823884454,-1.81144244019896));
#4346=CARTESIAN_POINT('Ctrl Pts',(14.8131130783409,-32.6447163505684,-2.15521684061908));
#4347=CARTESIAN_POINT('Ctrl Pts',(14.4942457593237,-33.0762503126915,-2.49899124103919));
#4348=CARTESIAN_POINT('Ctrl Pts',(14.0883919872725,-33.5580059268895,-2.59528770975726));
#4349=CARTESIAN_POINT('Ctrl Pts',(13.6825382152214,-34.0397615410876,-2.69158417847533));
#4350=CARTESIAN_POINT('Ctrl Pts',(13.291303264039,-34.5130769751218,-2.52133001886305));
#4351=CARTESIAN_POINT('Ctrl Pts',(12.9000683128565,-34.9863924091561,-2.35107585925076));
#4352=CARTESIAN_POINT('Ctrl Pts',(12.6221620196843,-35.3942775119812,-1.94799199564959));
#4353=CARTESIAN_POINT('Ctrl Pts',(12.3442557265121,-35.8021626148064,-1.54490813204841));
#4354=CARTESIAN_POINT('Ctrl Pts',(12.255941797888,-36.1005865149234,-0.988830267143717));
#4355=CARTESIAN_POINT('Ctrl Pts',(12.1676278692639,-36.3990104150405,-0.432752402239027));
#4356=CARTESIAN_POINT('Ctrl Pts',(12.3076189187291,-36.5656223746002,0.166181422977342));
#4357=CARTESIAN_POINT('Ctrl Pts',(12.4476099681944,-36.73223433416,0.765115248193711));
#4358=CARTESIAN_POINT('Ctrl Pts',(12.8094000084029,-36.7707905867082,1.28827884419634));
#4359=CARTESIAN_POINT('Ctrl Pts',(13.1711900486114,-36.8093468392564,1.81144244019896));
#4360=CARTESIAN_POINT('Ctrl Pts',(13.7043430819143,-36.7489666216124,2.15521684061908));
#4361=CARTESIAN_POINT('Ctrl Pts',(14.2374961152173,-36.6885864039684,2.49899124103919));
#4362=CARTESIAN_POINT('Ctrl Pts',(14.8576356015541,-36.5779845342494,2.59528770975726));
#4363=CARTESIAN_POINT('Ctrl Pts',(15.477775087891,-36.4673826645304,2.69158417847533));
#4364=CARTESIAN_POINT('Ctrl Pts',(16.0832957533591,-36.3652209749752,2.52133001886304));
#4365=CARTESIAN_POINT('Ctrl Pts',(16.6888164188273,-36.26305928542,2.35107585925076));
#4366=CARTESIAN_POINT('Ctrl Pts',(17.1810084262852,-36.2263279270739,1.94799199564959));
#4367=CARTESIAN_POINT('Ctrl Pts',(17.6732004337431,-36.1895965687278,1.54490813204841));
#4368=CARTESIAN_POINT('Ctrl Pts',(17.9758000766529,-36.2623264130898,0.988830267143717));
#4369=CARTESIAN_POINT('Ctrl Pts',(18.2783997195628,-36.3350562574518,0.432752402239027));
#4370=CARTESIAN_POINT('Ctrl Pts',(18.3526943843832,-36.539598042371,-0.166181422977342));
#4371=CARTESIAN_POINT('Ctrl Pts',(18.4269890492037,-36.7441398272903,-0.765115248193711));
#4372=CARTESIAN_POINT('Ctrl Pts',(18.2794847232809,-37.0767373192211,-1.28827884419634));
#4373=CARTESIAN_POINT('Ctrl Pts',(18.1319803973581,-37.409334811152,-1.81144244019896));
#4374=CARTESIAN_POINT('Ctrl Pts',(17.8131130783409,-37.8408687732751,-2.15521684061908));
#4375=CARTESIAN_POINT('Ctrl Pts',(17.4942457593237,-38.2724027353981,-2.49899124103919));
#4376=CARTESIAN_POINT('Ctrl Pts',(17.0883919872725,-38.7541583495962,-2.59528770975726));
#4377=CARTESIAN_POINT('Ctrl Pts',(16.6825382152214,-39.2359139637942,-2.69158417847533));
#4378=CARTESIAN_POINT('Ctrl Pts',(16.2913032640389,-39.7092293978285,-2.52133001886305));
#4379=CARTESIAN_POINT('Ctrl Pts',(15.9000683128565,-40.1825448318627,-2.35107585925076));
#4380=CARTESIAN_POINT('Ctrl Pts',(15.6221620196843,-40.5904299346879,-1.94799199564959));
#4381=CARTESIAN_POINT('Ctrl Pts',(15.3442557265121,-40.998315037513,-1.54490813204841));
#4382=CARTESIAN_POINT('Ctrl Pts',(15.255941797888,-41.2967389376301,-0.988830267143717));
#4383=CARTESIAN_POINT('Ctrl Pts',(15.1676278692638,-41.5951628377471,-0.432752402239027));
#4384=CARTESIAN_POINT('Ctrl Pts',(15.3076189187291,-41.7617747973069,0.166181422977342));
#4385=CARTESIAN_POINT('Ctrl Pts',(15.4476099681943,-41.9283867568667,0.765115248193711));
#4386=CARTESIAN_POINT('Ctrl Pts',(15.8094000084029,-41.9669430094149,1.28827884419634));
#4387=CARTESIAN_POINT('Ctrl Pts',(16.1711900486114,-42.0054992619631,1.81144244019896));
#4388=CARTESIAN_POINT('Ctrl Pts',(16.7043430819143,-41.945119044319,2.15521684061908));
#4389=CARTESIAN_POINT('Ctrl Pts',(17.2374961152172,-41.884738826675,2.49899124103919));
#4390=CARTESIAN_POINT('Ctrl Pts',(17.8576356015541,-41.774136956956,2.59528770975726));
#4391=CARTESIAN_POINT('Ctrl Pts',(18.4777750878909,-41.6635350872371,2.69158417847533));
#4392=CARTESIAN_POINT('Ctrl Pts',(19.0832957533591,-41.5613733976818,2.52133001886304));
#4393=CARTESIAN_POINT('Ctrl Pts',(19.6888164188272,-41.4592117081266,2.35107585925076));
#4394=CARTESIAN_POINT('Ctrl Pts',(20.1810084262851,-41.4224803497805,1.94799199564959));
#4395=CARTESIAN_POINT('Ctrl Pts',(20.673200433743,-41.3857489914344,1.54490813204841));
#4396=CARTESIAN_POINT('Ctrl Pts',(20.9758000766529,-41.4584788357964,0.988830267143717));
#4397=CARTESIAN_POINT('Ctrl Pts',(21.2783997195627,-41.5312086801584,0.432752402239027));
#4398=CARTESIAN_POINT('Ctrl Pts',(21.3526943843832,-41.7357504650777,-0.166181422977342));
#4399=CARTESIAN_POINT('Ctrl Pts',(21.4269890492037,-41.940292249997,-0.765115248193711));
#4400=CARTESIAN_POINT('Ctrl Pts',(21.2794847232809,-42.2728897419278,-1.28827884419634));
#4401=CARTESIAN_POINT('Ctrl Pts',(21.131980397358,-42.6054872338587,-1.81144244019896));
#4402=CARTESIAN_POINT('Ctrl Pts',(20.8131130783408,-43.0370211959817,-2.15521684061908));
#4403=CARTESIAN_POINT('Ctrl Pts',(20.4942457593236,-43.4685551581048,-2.49899124103919));
#4404=CARTESIAN_POINT('Ctrl Pts',(20.0883919872725,-43.9503107723028,-2.59528770975726));
#4405=CARTESIAN_POINT('Ctrl Pts',(19.6825382152213,-44.4320663865008,-2.69158417847533));
#4406=CARTESIAN_POINT('Ctrl Pts',(19.2913032640389,-44.9053818205351,-2.52133001886305));
#4407=CARTESIAN_POINT('Ctrl Pts',(18.9000683128565,-45.3786972545694,-2.35107585925076));
#4408=CARTESIAN_POINT('Ctrl Pts',(18.6221620196843,-45.7865823573945,-1.94799199564959));
#4409=CARTESIAN_POINT('Ctrl Pts',(4.55184415422078,-20.0688325405066,-1.69008569379309));
#4410=CARTESIAN_POINT('Ctrl Pts',(4.32491681918215,-20.4472849281303,-1.4407517010054));
#4411=CARTESIAN_POINT('Ctrl Pts',(4.22476116346577,-20.7525456525717,-1.04873843619563));
#4412=CARTESIAN_POINT('Ctrl Pts',(4.12460550774938,-21.0578063770131,-0.656725171385866));
#4413=CARTESIAN_POINT('Ctrl Pts',(4.19227954417643,-21.2661705835175,-0.199675669376779));
#4414=CARTESIAN_POINT('Ctrl Pts',(4.25995358060348,-21.4745347900219,0.257373832632308));
#4415=CARTESIAN_POINT('Ctrl Pts',(4.50327459317005,-21.5814891675698,0.688935312623524));
#4416=CARTESIAN_POINT('Ctrl Pts',(4.74659560573663,-21.6884435451177,1.12049679261474));
#4417=CARTESIAN_POINT('Ctrl Pts',(5.13859184064558,-21.7095602430244,1.44109420672161));
#4418=CARTESIAN_POINT('Ctrl Pts',(5.53058807555453,-21.7306769409311,1.76169162082848));
#4419=CARTESIAN_POINT('Ctrl Pts',(6.01484082784187,-21.6985293136949,1.90782671931788));
#4420=CARTESIAN_POINT('Ctrl Pts',(6.49909358012921,-21.6663816864587,2.05396181780729));
#4421=CARTESIAN_POINT('Ctrl Pts',(7.00091161011221,-21.6240927414165,1.99669075219403));
#4422=CARTESIAN_POINT('Ctrl Pts',(7.50272964009522,-21.5818037963743,1.93941968658077));
#4423=CARTESIAN_POINT('Ctrl Pts',(7.94394268941957,-21.5745051532296,1.69008569379309));
#4424=CARTESIAN_POINT('Ctrl Pts',(8.38515573874391,-21.5672065100849,1.4407517010054));
#4425=CARTESIAN_POINT('Ctrl Pts',(8.699597108746,-21.6330995301225,1.04873843619563));
#4426=CARTESIAN_POINT('Ctrl Pts',(9.0140384787481,-21.6989925501602,0.656725171385866));
#4427=CARTESIAN_POINT('Ctrl Pts',(9.16065015660677,-21.8617820881348,0.199675669376779));
#4428=CARTESIAN_POINT('Ctrl Pts',(9.30726183446543,-22.0245716261095,-0.257373832632308));
#4429=CARTESIAN_POINT('Ctrl Pts',(9.27822653618457,-22.2887709930406,-0.688935312623524));
#4430=CARTESIAN_POINT('Ctrl Pts',(9.24919123790371,-22.5529703599718,-1.12049679261474));
#4431=CARTESIAN_POINT('Ctrl Pts',(9.07148071728047,-22.9030074065441,-1.44109420672161));
#4432=CARTESIAN_POINT('Ctrl Pts',(8.89377019665723,-23.2530444531165,-1.76169162082848));
#4433=CARTESIAN_POINT('Ctrl Pts',(8.6238031586556,-23.6563458248317,-1.90782671931788));
#4434=CARTESIAN_POINT('Ctrl Pts',(8.35383612065398,-24.059647196547,-2.05396181780729));
#4435=CARTESIAN_POINT('Ctrl Pts',(8.06630380495668,-24.4730898860682,-1.99669075219403));
#4436=CARTESIAN_POINT('Ctrl Pts',(7.77877148925938,-24.8865325755895,-1.93941968658077));
#4437=CARTESIAN_POINT('Ctrl Pts',(7.55184415422075,-25.2649849632132,-1.69008569379309));
#4438=CARTESIAN_POINT('Ctrl Pts',(7.32491681918212,-25.6434373508369,-1.4407517010054));
#4439=CARTESIAN_POINT('Ctrl Pts',(7.22476116346574,-25.9486980752784,-1.04873843619563));
#4440=CARTESIAN_POINT('Ctrl Pts',(7.12460550774935,-26.2539587997198,-0.656725171385866));
#4441=CARTESIAN_POINT('Ctrl Pts',(7.1922795441764,-26.4623230062242,-0.199675669376779));
#4442=CARTESIAN_POINT('Ctrl Pts',(7.25995358060345,-26.6706872127285,0.257373832632308));
#4443=CARTESIAN_POINT('Ctrl Pts',(7.50327459317002,-26.7776415902764,0.688935312623524));
#4444=CARTESIAN_POINT('Ctrl Pts',(7.7465956057366,-26.8845959678243,1.12049679261474));
#4445=CARTESIAN_POINT('Ctrl Pts',(8.13859184064555,-26.905712665731,1.44109420672161));
#4446=CARTESIAN_POINT('Ctrl Pts',(8.5305880755545,-26.9268293636377,1.76169162082848));
#4447=CARTESIAN_POINT('Ctrl Pts',(9.01484082784184,-26.8946817364015,1.90782671931788));
#4448=CARTESIAN_POINT('Ctrl Pts',(9.49909358012917,-26.8625341091653,2.05396181780729));
#4449=CARTESIAN_POINT('Ctrl Pts',(10.0009116101122,-26.8202451641231,1.99669075219403));
#4450=CARTESIAN_POINT('Ctrl Pts',(10.5027296400952,-26.7779562190809,1.93941968658077));
#4451=CARTESIAN_POINT('Ctrl Pts',(10.9439426894195,-26.7706575759362,1.69008569379309));
#4452=CARTESIAN_POINT('Ctrl Pts',(11.3851557387439,-26.7633589327915,1.4407517010054));
#4453=CARTESIAN_POINT('Ctrl Pts',(11.699597108746,-26.8292519528292,1.04873843619563));
#4454=CARTESIAN_POINT('Ctrl Pts',(12.0140384787481,-26.8951449728668,0.656725171385866));
#4455=CARTESIAN_POINT('Ctrl Pts',(12.1606501566067,-27.0579345108415,0.199675669376779));
#4456=CARTESIAN_POINT('Ctrl Pts',(12.3072618344654,-27.2207240488161,-0.257373832632308));
#4457=CARTESIAN_POINT('Ctrl Pts',(12.2782265361845,-27.4849234157473,-0.688935312623524));
#4458=CARTESIAN_POINT('Ctrl Pts',(12.2491912379037,-27.7491227826784,-1.12049679261474));
#4459=CARTESIAN_POINT('Ctrl Pts',(12.0714807172804,-28.0991598292508,-1.44109420672161));
#4460=CARTESIAN_POINT('Ctrl Pts',(11.8937701966572,-28.4491968758231,-1.76169162082848));
#4461=CARTESIAN_POINT('Ctrl Pts',(11.6238031586556,-28.8524982475384,-1.90782671931788));
#4462=CARTESIAN_POINT('Ctrl Pts',(11.3538361206539,-29.2557996192536,-2.05396181780729));
#4463=CARTESIAN_POINT('Ctrl Pts',(11.0663038049567,-29.6692423087749,-1.99669075219403));
#4464=CARTESIAN_POINT('Ctrl Pts',(10.7787714892594,-30.0826849982961,-1.93941968658077));
#4465=CARTESIAN_POINT('Ctrl Pts',(10.5518441542207,-30.4611373859199,-1.69008569379309));
#4466=CARTESIAN_POINT('Ctrl Pts',(10.3249168191821,-30.8395897735436,-1.4407517010054));
#4467=CARTESIAN_POINT('Ctrl Pts',(10.2247611634657,-31.144850497985,-1.04873843619563));
#4468=CARTESIAN_POINT('Ctrl Pts',(10.1246055077493,-31.4501112224264,-0.656725171385866));
#4469=CARTESIAN_POINT('Ctrl Pts',(10.1922795441764,-31.6584754289308,-0.199675669376779));
#4470=CARTESIAN_POINT('Ctrl Pts',(10.2599535806034,-31.8668396354352,0.257373832632308));
#4471=CARTESIAN_POINT('Ctrl Pts',(10.50327459317,-31.9737940129831,0.688935312623524));
#4472=CARTESIAN_POINT('Ctrl Pts',(10.7465956057366,-32.080748390531,1.12049679261474));
#4473=CARTESIAN_POINT('Ctrl Pts',(11.1385918406455,-32.1018650884377,1.44109420672161));
#4474=CARTESIAN_POINT('Ctrl Pts',(11.5305880755545,-32.1229817863444,1.76169162082848));
#4475=CARTESIAN_POINT('Ctrl Pts',(12.0148408278418,-32.0908341591082,1.90782671931788));
#4476=CARTESIAN_POINT('Ctrl Pts',(12.4990935801291,-32.0586865318719,2.05396181780729));
#4477=CARTESIAN_POINT('Ctrl Pts',(13.0009116101121,-32.0163975868298,1.99669075219403));
#4478=CARTESIAN_POINT('Ctrl Pts',(13.5027296400952,-31.9741086417876,1.93941968658077));
#4479=CARTESIAN_POINT('Ctrl Pts',(13.9439426894195,-31.9668099986429,1.69008569379309));
#4480=CARTESIAN_POINT('Ctrl Pts',(14.3851557387438,-31.9595113554982,1.4407517010054));
#4481=CARTESIAN_POINT('Ctrl Pts',(14.6995971087459,-32.0254043755358,1.04873843619563));
#4482=CARTESIAN_POINT('Ctrl Pts',(15.014038478748,-32.0912973955735,0.656725171385866));
#4483=CARTESIAN_POINT('Ctrl Pts',(15.1606501566067,-32.2540869335481,0.199675669376779));
#4484=CARTESIAN_POINT('Ctrl Pts',(15.3072618344654,-32.4168764715228,-0.257373832632308));
#4485=CARTESIAN_POINT('Ctrl Pts',(15.2782265361845,-32.6810758384539,-0.688935312623524));
#4486=CARTESIAN_POINT('Ctrl Pts',(15.2491912379036,-32.9452752053851,-1.12049679261474));
#4487=CARTESIAN_POINT('Ctrl Pts',(15.0714807172804,-33.2953122519574,-1.44109420672161));
#4488=CARTESIAN_POINT('Ctrl Pts',(14.8937701966572,-33.6453492985298,-1.76169162082848));
#4489=CARTESIAN_POINT('Ctrl Pts',(14.6238031586555,-34.048650670245,-1.90782671931788));
#4490=CARTESIAN_POINT('Ctrl Pts',(14.3538361206539,-34.4519520419603,-2.05396181780729));
#4491=CARTESIAN_POINT('Ctrl Pts',(14.0663038049566,-34.8653947314815,-1.99669075219403));
#4492=CARTESIAN_POINT('Ctrl Pts',(13.7787714892593,-35.2788374210028,-1.93941968658077));
#4493=CARTESIAN_POINT('Ctrl Pts',(13.5518441542207,-35.6572898086265,-1.69008569379309));
#4494=CARTESIAN_POINT('Ctrl Pts',(13.3249168191821,-36.0357421962502,-1.4407517010054));
#4495=CARTESIAN_POINT('Ctrl Pts',(13.2247611634657,-36.3410029206916,-1.04873843619563));
#4496=CARTESIAN_POINT('Ctrl Pts',(13.1246055077493,-36.6462636451331,-0.656725171385866));
#4497=CARTESIAN_POINT('Ctrl Pts',(13.1922795441763,-36.8546278516375,-0.199675669376779));
#4498=CARTESIAN_POINT('Ctrl Pts',(13.2599535806034,-37.0629920581418,0.257373832632308));
#4499=CARTESIAN_POINT('Ctrl Pts',(13.50327459317,-37.1699464356897,0.688935312623524));
#4500=CARTESIAN_POINT('Ctrl Pts',(13.7465956057365,-37.2769008132376,1.12049679261474));
#4501=CARTESIAN_POINT('Ctrl Pts',(14.1385918406455,-37.2980175111443,1.44109420672161));
#4502=CARTESIAN_POINT('Ctrl Pts',(14.5305880755544,-37.319134209051,1.76169162082848));
#4503=CARTESIAN_POINT('Ctrl Pts',(15.0148408278418,-37.2869865818148,1.90782671931788));
#4504=CARTESIAN_POINT('Ctrl Pts',(15.4990935801291,-37.2548389545786,2.05396181780729));
#4505=CARTESIAN_POINT('Ctrl Pts',(16.0009116101121,-37.2125500095364,1.99669075219403));
#4506=CARTESIAN_POINT('Ctrl Pts',(16.5027296400951,-37.1702610644942,1.93941968658077));
#4507=CARTESIAN_POINT('Ctrl Pts',(16.9439426894195,-37.1629624213495,1.69008569379309));
#4508=CARTESIAN_POINT('Ctrl Pts',(17.3851557387438,-37.1556637782049,1.4407517010054));
#4509=CARTESIAN_POINT('Ctrl Pts',(17.6995971087459,-37.2215567982425,1.04873843619563));
#4510=CARTESIAN_POINT('Ctrl Pts',(18.014038478748,-37.2874498182801,0.656725171385866));
#4511=CARTESIAN_POINT('Ctrl Pts',(18.1606501566067,-37.4502393562548,0.199675669376779));
#4512=CARTESIAN_POINT('Ctrl Pts',(18.3072618344653,-37.6130288942294,-0.257373832632308));
#4513=CARTESIAN_POINT('Ctrl Pts',(18.2782265361845,-37.8772282611606,-0.688935312623524));
#4514=CARTESIAN_POINT('Ctrl Pts',(18.2491912379036,-38.1414276280917,-1.12049679261474));
#4515=CARTESIAN_POINT('Ctrl Pts',(18.0714807172804,-38.4914646746641,-1.44109420672161));
#4516=CARTESIAN_POINT('Ctrl Pts',(17.8937701966571,-38.8415017212364,-1.76169162082848));
#4517=CARTESIAN_POINT('Ctrl Pts',(17.6238031586555,-39.2448030929517,-1.90782671931788));
#4518=CARTESIAN_POINT('Ctrl Pts',(17.3538361206539,-39.6481044646669,-2.05396181780729));
#4519=CARTESIAN_POINT('Ctrl Pts',(17.0663038049566,-40.0615471541882,-1.99669075219403));
#4520=CARTESIAN_POINT('Ctrl Pts',(16.7787714892593,-40.4749898437094,-1.93941968658077));
#4521=CARTESIAN_POINT('Ctrl Pts',(16.5518441542207,-40.8534422313332,-1.69008569379309));
#4522=CARTESIAN_POINT('Ctrl Pts',(16.324916819182,-41.2318946189569,-1.4407517010054));
#4523=CARTESIAN_POINT('Ctrl Pts',(16.2247611634656,-41.5371553433983,-1.04873843619563));
#4524=CARTESIAN_POINT('Ctrl Pts',(16.1246055077493,-41.8424160678397,-0.656725171385866));
#4525=CARTESIAN_POINT('Ctrl Pts',(16.1922795441763,-42.0507802743441,-0.199675669376779));
#4526=CARTESIAN_POINT('Ctrl Pts',(16.2599535806034,-42.2591444808485,0.257373832632308));
#4527=CARTESIAN_POINT('Ctrl Pts',(16.5032745931699,-42.3660988583964,0.688935312623524));
#4528=CARTESIAN_POINT('Ctrl Pts',(16.7465956057365,-42.4730532359443,1.12049679261474));
#4529=CARTESIAN_POINT('Ctrl Pts',(17.1385918406455,-42.494169933851,1.44109420672161));
#4530=CARTESIAN_POINT('Ctrl Pts',(17.5305880755544,-42.5152866317577,1.76169162082848));
#4531=CARTESIAN_POINT('Ctrl Pts',(18.0148408278417,-42.4831390045215,1.90782671931788));
#4532=CARTESIAN_POINT('Ctrl Pts',(18.4990935801291,-42.4509913772853,2.05396181780729));
#4533=CARTESIAN_POINT('Ctrl Pts',(19.0009116101121,-42.4087024322431,1.99669075219403));
#4534=CARTESIAN_POINT('Ctrl Pts',(19.5027296400951,-42.3664134872009,1.93941968658077));
#4535=CARTESIAN_POINT('Ctrl Pts',(19.9439426894194,-42.3591148440562,1.69008569379309));
#4536=CARTESIAN_POINT('Ctrl Pts',(20.3851557387438,-42.3518162009115,1.4407517010054));
#4537=CARTESIAN_POINT('Ctrl Pts',(20.6995971087459,-42.4177092209491,1.04873843619563));
#4538=CARTESIAN_POINT('Ctrl Pts',(21.014038478748,-42.4836022409868,0.656725171385866));
#4539=CARTESIAN_POINT('Ctrl Pts',(21.1606501566066,-42.6463917789614,0.199675669376779));
#4540=CARTESIAN_POINT('Ctrl Pts',(21.3072618344653,-42.8091813169361,-0.257373832632308));
#4541=CARTESIAN_POINT('Ctrl Pts',(21.2782265361844,-43.0733806838672,-0.688935312623524));
#4542=CARTESIAN_POINT('Ctrl Pts',(21.2491912379036,-43.3375800507984,-1.12049679261474));
#4543=CARTESIAN_POINT('Ctrl Pts',(21.0714807172803,-43.6876170973707,-1.44109420672161));
#4544=CARTESIAN_POINT('Ctrl Pts',(20.8937701966571,-44.0376541439431,-1.76169162082848));
#4545=CARTESIAN_POINT('Ctrl Pts',(20.6238031586555,-44.4409555156583,-1.90782671931788));
#4546=CARTESIAN_POINT('Ctrl Pts',(20.3538361206538,-44.8442568873736,-2.05396181780729));
#4547=CARTESIAN_POINT('Ctrl Pts',(20.0663038049566,-45.2576995768948,-1.99669075219403));
#4548=CARTESIAN_POINT('Ctrl Pts',(19.7787714892593,-45.6711422664161,-1.93941968658077));
#4549=CARTESIAN_POINT('Ctrl Pts',(19.5518441542206,-46.0495946540398,-1.69008569379309));
#4550=CARTESIAN_POINT('Ctrl Pts',(4.55184415422078,-19.3686903861425,-0.976082217833403));
#4551=CARTESIAN_POINT('Ctrl Pts',(4.4660500642644,-19.6656594567264,-0.80664966398524));
#4552=CARTESIAN_POINT('Ctrl Pts',(4.46302775611024,-19.9148402168055,-0.557333680706485));
#4553=CARTESIAN_POINT('Ctrl Pts',(4.46000544795609,-20.1640209768846,-0.30801769742773));
#4554=CARTESIAN_POINT('Ctrl Pts',(4.56157448367832,-20.3528158964217,-0.0281983728666175));
#4555=CARTESIAN_POINT('Ctrl Pts',(4.66314351940055,-20.5416108159588,0.251620951694495));
#4556=CARTESIAN_POINT('Ctrl Pts',(4.87040786268996,-20.66938252122,0.506521968549832));
#4557=CARTESIAN_POINT('Ctrl Pts',(5.07767220597936,-20.7971542264811,0.761422985405168));
#4558=CARTESIAN_POINT('Ctrl Pts',(5.37080156859517,-20.8753517397202,0.940919422010711));
#4559=CARTESIAN_POINT('Ctrl Pts',(5.66393093121099,-20.9535492529593,1.12041585861625));
#4560=CARTESIAN_POINT('Ctrl Pts',(6.00608840476948,-21.0034403731477,1.18895624432295));
#4561=CARTESIAN_POINT('Ctrl Pts',(6.34824587832798,-21.0533314933362,1.25749663002964));
#4562=CARTESIAN_POINT('Ctrl Pts',(6.69288393578292,-21.1017904477443,1.2015057008556));
#4563=CARTESIAN_POINT('Ctrl Pts',(7.03752199323787,-21.1502494021524,1.14551477168157));
#4564=CARTESIAN_POINT('Ctrl Pts',(7.33760179747996,-21.2244340760476,0.976082217833403));
#4565=CARTESIAN_POINT('Ctrl Pts',(7.63768160172206,-21.2986187499427,0.80664966398524));
#4566=CARTESIAN_POINT('Ctrl Pts',(7.85498962416192,-21.4205917343427,0.557333680706485));
#4567=CARTESIAN_POINT('Ctrl Pts',(8.07229764660179,-21.5425647187427,0.308017697427731));
#4568=CARTESIAN_POINT('Ctrl Pts',(8.18501432516527,-21.7249235436846,0.0281983728666177));
#4569=CARTESIAN_POINT('Ctrl Pts',(8.29773100372875,-21.9072823686265,-0.251620951694495));
#4570=CARTESIAN_POINT('Ctrl Pts',(8.30475237472506,-22.1506644078444,-0.506521968549832));
#4571=CARTESIAN_POINT('Ctrl Pts',(8.31177374572137,-22.3940464470623,-0.761422985405168));
#4572=CARTESIAN_POINT('Ctrl Pts',(8.23293009739127,-22.6870026783022,-0.940919422010711));
#4573=CARTESIAN_POINT('Ctrl Pts',(8.15408644906117,-22.9799589095422,-1.12041585861625));
#4574=CARTESIAN_POINT('Ctrl Pts',(8.02621468978838,-23.3012215338328,-1.18895624432295));
#4575=CARTESIAN_POINT('Ctrl Pts',(7.8983429305156,-23.6224841581234,-1.25749663002964));
#4576=CARTESIAN_POINT('Ctrl Pts',(7.76799058734637,-23.9451789481943,-1.2015057008556));
#4577=CARTESIAN_POINT('Ctrl Pts',(7.63763824417713,-24.2678737382653,-1.14551477168157));
#4578=CARTESIAN_POINT('Ctrl Pts',(7.55184415422075,-24.5648428088492,-0.976082217833403));
#4579=CARTESIAN_POINT('Ctrl Pts',(7.46605006426437,-24.8618118794331,-0.80664966398524));
#4580=CARTESIAN_POINT('Ctrl Pts',(7.46302775611021,-25.1109926395121,-0.557333680706485));
#4581=CARTESIAN_POINT('Ctrl Pts',(7.46000544795606,-25.3601733995912,-0.30801769742773));
#4582=CARTESIAN_POINT('Ctrl Pts',(7.56157448367829,-25.5489683191283,-0.0281983728666175));
#4583=CARTESIAN_POINT('Ctrl Pts',(7.66314351940052,-25.7377632386655,0.251620951694495));
#4584=CARTESIAN_POINT('Ctrl Pts',(7.87040786268992,-25.8655349439266,0.506521968549832));
#4585=CARTESIAN_POINT('Ctrl Pts',(8.07767220597933,-25.9933066491878,0.761422985405168));
#4586=CARTESIAN_POINT('Ctrl Pts',(8.37080156859514,-26.0715041624269,0.940919422010711));
#4587=CARTESIAN_POINT('Ctrl Pts',(8.66393093121095,-26.1497016756659,1.12041585861625));
#4588=CARTESIAN_POINT('Ctrl Pts',(9.00608840476945,-26.1995927958544,1.18895624432295));
#4589=CARTESIAN_POINT('Ctrl Pts',(9.34824587832795,-26.2494839160429,1.25749663002964));
#4590=CARTESIAN_POINT('Ctrl Pts',(9.69288393578289,-26.297942870451,1.2015057008556));
#4591=CARTESIAN_POINT('Ctrl Pts',(10.0375219932378,-26.346401824859,1.14551477168157));
#4592=CARTESIAN_POINT('Ctrl Pts',(10.3376017974799,-26.4205864987542,0.976082217833403));
#4593=CARTESIAN_POINT('Ctrl Pts',(10.637681601722,-26.4947711726494,0.80664966398524));
#4594=CARTESIAN_POINT('Ctrl Pts',(10.8549896241619,-26.6167441570493,0.557333680706485));
#4595=CARTESIAN_POINT('Ctrl Pts',(11.0722976466018,-26.7387171414493,0.308017697427731));
#4596=CARTESIAN_POINT('Ctrl Pts',(11.1850143251652,-26.9210759663912,0.0281983728666177));
#4597=CARTESIAN_POINT('Ctrl Pts',(11.2977310037287,-27.1034347913331,-0.251620951694495));
#4598=CARTESIAN_POINT('Ctrl Pts',(11.304752374725,-27.346816830551,-0.506521968549832));
#4599=CARTESIAN_POINT('Ctrl Pts',(11.3117737457213,-27.5901988697689,-0.761422985405168));
#4600=CARTESIAN_POINT('Ctrl Pts',(11.2329300973912,-27.8831551010089,-0.940919422010711));
#4601=CARTESIAN_POINT('Ctrl Pts',(11.1540864490611,-28.1761113322489,-1.12041585861625));
#4602=CARTESIAN_POINT('Ctrl Pts',(11.0262146897884,-28.4973739565395,-1.18895624432295));
#4603=CARTESIAN_POINT('Ctrl Pts',(10.8983429305156,-28.8186365808301,-1.25749663002964));
#4604=CARTESIAN_POINT('Ctrl Pts',(10.7679905873463,-29.141331370901,-1.2015057008556));
#4605=CARTESIAN_POINT('Ctrl Pts',(10.6376382441771,-29.4640261609719,-1.14551477168157));
#4606=CARTESIAN_POINT('Ctrl Pts',(10.5518441542207,-29.7609952315558,-0.976082217833403));
#4607=CARTESIAN_POINT('Ctrl Pts',(10.4660500642643,-30.0579643021397,-0.80664966398524));
#4608=CARTESIAN_POINT('Ctrl Pts',(10.4630277561102,-30.3071450622188,-0.557333680706485));
#4609=CARTESIAN_POINT('Ctrl Pts',(10.460005447956,-30.5563258222979,-0.30801769742773));
#4610=CARTESIAN_POINT('Ctrl Pts',(10.5615744836783,-30.745120741835,-0.0281983728666175));
#4611=CARTESIAN_POINT('Ctrl Pts',(10.6631435194005,-30.9339156613721,0.251620951694495));
#4612=CARTESIAN_POINT('Ctrl Pts',(10.8704078626899,-31.0616873666333,0.506521968549832));
#4613=CARTESIAN_POINT('Ctrl Pts',(11.0776722059793,-31.1894590718944,0.761422985405168));
#4614=CARTESIAN_POINT('Ctrl Pts',(11.3708015685951,-31.2676565851335,0.940919422010711));
#4615=CARTESIAN_POINT('Ctrl Pts',(11.6639309312109,-31.3458540983726,1.12041585861625));
#4616=CARTESIAN_POINT('Ctrl Pts',(12.0060884047694,-31.395745218561,1.18895624432295));
#4617=CARTESIAN_POINT('Ctrl Pts',(12.3482458783279,-31.4456363387495,1.25749663002964));
#4618=CARTESIAN_POINT('Ctrl Pts',(12.6928839357829,-31.4940952931576,1.2015057008556));
#4619=CARTESIAN_POINT('Ctrl Pts',(13.0375219932378,-31.5425542475657,1.14551477168157));
#4620=CARTESIAN_POINT('Ctrl Pts',(13.3376017974799,-31.6167389214609,0.976082217833403));
#4621=CARTESIAN_POINT('Ctrl Pts',(13.637681601722,-31.690923595356,0.80664966398524));
#4622=CARTESIAN_POINT('Ctrl Pts',(13.8549896241619,-31.812896579756,0.557333680706485));
#4623=CARTESIAN_POINT('Ctrl Pts',(14.0722976466017,-31.934869564156,0.308017697427731));
#4624=CARTESIAN_POINT('Ctrl Pts',(14.1850143251652,-32.1172283890979,0.0281983728666177));
#4625=CARTESIAN_POINT('Ctrl Pts',(14.2977310037287,-32.2995872140398,-0.251620951694495));
#4626=CARTESIAN_POINT('Ctrl Pts',(14.304752374725,-32.5429692532577,-0.506521968549832));
#4627=CARTESIAN_POINT('Ctrl Pts',(14.3117737457213,-32.7863512924756,-0.761422985405168));
#4628=CARTESIAN_POINT('Ctrl Pts',(14.2329300973912,-33.0793075237155,-0.940919422010711));
#4629=CARTESIAN_POINT('Ctrl Pts',(14.1540864490611,-33.3722637549555,-1.12041585861625));
#4630=CARTESIAN_POINT('Ctrl Pts',(14.0262146897883,-33.6935263792461,-1.18895624432295));
#4631=CARTESIAN_POINT('Ctrl Pts',(13.8983429305155,-34.0147890035367,-1.25749663002964));
#4632=CARTESIAN_POINT('Ctrl Pts',(13.7679905873463,-34.3374837936076,-1.2015057008556));
#4633=CARTESIAN_POINT('Ctrl Pts',(13.6376382441771,-34.6601785836786,-1.14551477168157));
#4634=CARTESIAN_POINT('Ctrl Pts',(13.5518441542207,-34.9571476542625,-0.976082217833403));
#4635=CARTESIAN_POINT('Ctrl Pts',(13.4660500642643,-35.2541167248464,-0.80664966398524));
#4636=CARTESIAN_POINT('Ctrl Pts',(13.4630277561101,-35.5032974849254,-0.557333680706485));
#4637=CARTESIAN_POINT('Ctrl Pts',(13.460005447956,-35.7524782450045,-0.30801769742773));
#4638=CARTESIAN_POINT('Ctrl Pts',(13.5615744836782,-35.9412731645416,-0.0281983728666175));
#4639=CARTESIAN_POINT('Ctrl Pts',(13.6631435194005,-36.1300680840788,0.251620951694495));
#4640=CARTESIAN_POINT('Ctrl Pts',(13.8704078626899,-36.2578397893399,0.506521968549832));
#4641=CARTESIAN_POINT('Ctrl Pts',(14.0776722059793,-36.3856114946011,0.761422985405168));
#4642=CARTESIAN_POINT('Ctrl Pts',(14.3708015685951,-36.4638090078402,0.940919422010711));
#4643=CARTESIAN_POINT('Ctrl Pts',(14.6639309312109,-36.5420065210792,1.12041585861625));
#4644=CARTESIAN_POINT('Ctrl Pts',(15.0060884047694,-36.5918976412677,1.18895624432295));
#4645=CARTESIAN_POINT('Ctrl Pts',(15.3482458783279,-36.6417887614562,1.25749663002964));
#4646=CARTESIAN_POINT('Ctrl Pts',(15.6928839357828,-36.6902477158643,1.2015057008556));
#4647=CARTESIAN_POINT('Ctrl Pts',(16.0375219932378,-36.7387066702723,1.14551477168157));
#4648=CARTESIAN_POINT('Ctrl Pts',(16.3376017974799,-36.8128913441675,0.976082217833403));
#4649=CARTESIAN_POINT('Ctrl Pts',(16.637681601722,-36.8870760180627,0.80664966398524));
#4650=CARTESIAN_POINT('Ctrl Pts',(16.8549896241618,-37.0090490024626,0.557333680706485));
#4651=CARTESIAN_POINT('Ctrl Pts',(17.0722976466017,-37.1310219868626,0.308017697427731));
#4652=CARTESIAN_POINT('Ctrl Pts',(17.1850143251652,-37.3133808118045,0.0281983728666177));
#4653=CARTESIAN_POINT('Ctrl Pts',(17.2977310037287,-37.4957396367464,-0.251620951694495));
#4654=CARTESIAN_POINT('Ctrl Pts',(17.304752374725,-37.7391216759643,-0.506521968549832));
#4655=CARTESIAN_POINT('Ctrl Pts',(17.3117737457213,-37.9825037151822,-0.761422985405168));
#4656=CARTESIAN_POINT('Ctrl Pts',(17.2329300973912,-38.2754599464222,-0.940919422010711));
#4657=CARTESIAN_POINT('Ctrl Pts',(17.1540864490611,-38.5684161776622,-1.12041585861625));
#4658=CARTESIAN_POINT('Ctrl Pts',(17.0262146897883,-38.8896788019527,-1.18895624432295));
#4659=CARTESIAN_POINT('Ctrl Pts',(16.8983429305155,-39.2109414262433,-1.25749663002964));
#4660=CARTESIAN_POINT('Ctrl Pts',(16.7679905873463,-39.5336362163143,-1.2015057008556));
#4661=CARTESIAN_POINT('Ctrl Pts',(16.637638244177,-39.8563310063852,-1.14551477168157));
#4662=CARTESIAN_POINT('Ctrl Pts',(16.5518441542207,-40.1533000769691,-0.976082217833403));
#4663=CARTESIAN_POINT('Ctrl Pts',(16.4660500642643,-40.450269147553,-0.80664966398524));
#4664=CARTESIAN_POINT('Ctrl Pts',(16.4630277561101,-40.6994499076321,-0.557333680706485));
#4665=CARTESIAN_POINT('Ctrl Pts',(16.460005447956,-40.9486306677112,-0.30801769742773));
#4666=CARTESIAN_POINT('Ctrl Pts',(16.5615744836782,-41.1374255872483,-0.0281983728666175));
#4667=CARTESIAN_POINT('Ctrl Pts',(16.6631435194004,-41.3262205067854,0.251620951694495));
#4668=CARTESIAN_POINT('Ctrl Pts',(16.8704078626898,-41.4539922120466,0.506521968549832));
#4669=CARTESIAN_POINT('Ctrl Pts',(17.0776722059792,-41.5817639173077,0.761422985405168));
#4670=CARTESIAN_POINT('Ctrl Pts',(17.370801568595,-41.6599614305468,0.940919422010711));
#4671=CARTESIAN_POINT('Ctrl Pts',(17.6639309312109,-41.7381589437859,1.12041585861625));
#4672=CARTESIAN_POINT('Ctrl Pts',(18.0060884047694,-41.7880500639744,1.18895624432295));
#4673=CARTESIAN_POINT('Ctrl Pts',(18.3482458783279,-41.8379411841628,1.25749663002964));
#4674=CARTESIAN_POINT('Ctrl Pts',(18.6928839357828,-41.8864001385709,1.2015057008556));
#4675=CARTESIAN_POINT('Ctrl Pts',(19.0375219932377,-41.934859092979,1.14551477168157));
#4676=CARTESIAN_POINT('Ctrl Pts',(19.3376017974798,-42.0090437668742,0.976082217833403));
#4677=CARTESIAN_POINT('Ctrl Pts',(19.6376816017219,-42.0832284407693,0.80664966398524));
#4678=CARTESIAN_POINT('Ctrl Pts',(19.8549896241618,-42.2052014251693,0.557333680706485));
#4679=CARTESIAN_POINT('Ctrl Pts',(20.0722976466017,-42.3271744095693,0.308017697427731));
#4680=CARTESIAN_POINT('Ctrl Pts',(20.1850143251651,-42.5095332345112,0.0281983728666177));
#4681=CARTESIAN_POINT('Ctrl Pts',(20.2977310037286,-42.6918920594531,-0.251620951694495));
#4682=CARTESIAN_POINT('Ctrl Pts',(20.3047523747249,-42.935274098671,-0.506521968549832));
#4683=CARTESIAN_POINT('Ctrl Pts',(20.3117737457212,-43.1786561378889,-0.761422985405168));
#4684=CARTESIAN_POINT('Ctrl Pts',(20.2329300973911,-43.4716123691288,-0.940919422010711));
#4685=CARTESIAN_POINT('Ctrl Pts',(20.154086449061,-43.7645686003688,-1.12041585861625));
#4686=CARTESIAN_POINT('Ctrl Pts',(20.0262146897883,-44.0858312246594,-1.18895624432295));
#4687=CARTESIAN_POINT('Ctrl Pts',(19.8983429305155,-44.40709384895,-1.25749663002964));
#4688=CARTESIAN_POINT('Ctrl Pts',(19.7679905873462,-44.7297886390209,-1.2015057008556));
#4689=CARTESIAN_POINT('Ctrl Pts',(19.637638244177,-45.0524834290919,-1.14551477168157));
#4690=CARTESIAN_POINT('Ctrl Pts',(19.5518441542206,-45.3494524996758,-0.976082217833403));
#4691=CARTESIAN_POINT('Ctrl Pts',(3.62216201968442,-19.1056780894973,-1.2339885196899));
#4692=CARTESIAN_POINT('Ctrl Pts',(3.48538897159447,-19.4320798752826,-0.910806095028249));
#4693=CARTESIAN_POINT('Ctrl Pts',(3.49420839053257,-19.6744238110373,-0.497425511654571));
#4694=CARTESIAN_POINT('Ctrl Pts',(3.50302780947066,-19.916767746792,-0.0840449282808927));
#4695=CARTESIAN_POINT('Ctrl Pts',(3.67691385823109,-20.0638104193845,0.337658719487502));
#4696=CARTESIAN_POINT('Ctrl Pts',(3.85079990699151,-20.2108530919771,0.759362367255897));
#4697=CARTESIAN_POINT('Ctrl Pts',(4.17653327792288,-20.2702266722385,1.10586550012264));
#4698=CARTESIAN_POINT('Ctrl Pts',(4.50226664885425,-20.3296002524999,1.45236863298939));
#4699=CARTESIAN_POINT('Ctrl Pts',(4.93655280986403,-20.3263008501883,1.65504205590818));
#4700=CARTESIAN_POINT('Ctrl Pts',(5.3708389708738,-20.3230014478767,1.85771547882697));
#4701=CARTESIAN_POINT('Ctrl Pts',(5.84888317848182,-20.2944383255823,1.87641723476232));
#4702=CARTESIAN_POINT('Ctrl Pts',(6.32692738608983,-20.265875203288,1.89511899069768));
#4703=CARTESIAN_POINT('Ctrl Pts',(6.77526807902992,-20.2544614131831,1.72614496752462));
#4704=CARTESIAN_POINT('Ctrl Pts',(7.22360877197,-20.2430476230782,1.55717094435156));
#4705=CARTESIAN_POINT('Ctrl Pts',(7.57466753434566,-20.2877995817719,1.2339885196899));
#4706=CARTESIAN_POINT('Ctrl Pts',(7.92572629672132,-20.3325515404656,0.910806095028249));
#4707=CARTESIAN_POINT('Ctrl Pts',(8.13119259206894,-20.46136134919,0.497425511654571));
#4708=CARTESIAN_POINT('Ctrl Pts',(8.33665888741656,-20.5901711579143,0.084044928280893));
#4709=CARTESIAN_POINT('Ctrl Pts',(8.37705855294184,-20.8142822298008,-0.337658719487502));
#4710=CARTESIAN_POINT('Ctrl Pts',(8.41745821846713,-21.0383933016873,-0.759362367255897));
#4711=CARTESIAN_POINT('Ctrl Pts',(8.30601056182147,-21.350173465905,-1.10586550012264));
#4712=CARTESIAN_POINT('Ctrl Pts',(8.19456290517582,-21.6619536301226,-1.45236863298939));
#4713=CARTESIAN_POINT('Ctrl Pts',(7.97456245845175,-22.0364067769132,-1.65504205590818));
#4714=CARTESIAN_POINT('Ctrl Pts',(7.75456201172769,-22.4108599237039,-1.85771547882697));
#4715=CARTESIAN_POINT('Ctrl Pts',(7.49080351840538,-22.8105767904773,-1.87641723476232));
#4716=CARTESIAN_POINT('Ctrl Pts',(7.22704502508308,-23.2102936572507,-1.89511899069768));
#4717=CARTESIAN_POINT('Ctrl Pts',(6.99299004642871,-23.5928611918346,-1.72614496752462));
#4718=CARTESIAN_POINT('Ctrl Pts',(6.75893506777434,-23.9754287264186,-1.55717094435156));
#4719=CARTESIAN_POINT('Ctrl Pts',(6.62216201968439,-24.3018305122039,-1.2339885196899));
#4720=CARTESIAN_POINT('Ctrl Pts',(6.48538897159444,-24.6282322979892,-0.910806095028249));
#4721=CARTESIAN_POINT('Ctrl Pts',(6.49420839053254,-24.8705762337439,-0.497425511654571));
#4722=CARTESIAN_POINT('Ctrl Pts',(6.50302780947063,-25.1129201694986,-0.0840449282808927));
#4723=CARTESIAN_POINT('Ctrl Pts',(6.67691385823105,-25.2599628420912,0.337658719487502));
#4724=CARTESIAN_POINT('Ctrl Pts',(6.85079990699148,-25.4070055146837,0.759362367255897));
#4725=CARTESIAN_POINT('Ctrl Pts',(7.17653327792285,-25.4663790949451,1.10586550012264));
#4726=CARTESIAN_POINT('Ctrl Pts',(7.50226664885422,-25.5257526752066,1.45236863298939));
#4727=CARTESIAN_POINT('Ctrl Pts',(7.936552809864,-25.5224532728949,1.65504205590818));
#4728=CARTESIAN_POINT('Ctrl Pts',(8.37083897087377,-25.5191538705833,1.85771547882697));
#4729=CARTESIAN_POINT('Ctrl Pts',(8.84888317848179,-25.490590748289,1.87641723476232));
#4730=CARTESIAN_POINT('Ctrl Pts',(9.3269273860898,-25.4620276259946,1.89511899069768));
#4731=CARTESIAN_POINT('Ctrl Pts',(9.77526807902988,-25.4506138358897,1.72614496752462));
#4732=CARTESIAN_POINT('Ctrl Pts',(10.22360877197,-25.4392000457848,1.55717094435156));
#4733=CARTESIAN_POINT('Ctrl Pts',(10.5746675343456,-25.4839520044785,1.2339885196899));
#4734=CARTESIAN_POINT('Ctrl Pts',(10.9257262967213,-25.5287039631723,0.910806095028249));
#4735=CARTESIAN_POINT('Ctrl Pts',(11.1311925920689,-25.6575137718966,0.497425511654571));
#4736=CARTESIAN_POINT('Ctrl Pts',(11.3366588874165,-25.786323580621,0.084044928280893));
#4737=CARTESIAN_POINT('Ctrl Pts',(11.3770585529418,-26.0104346525075,-0.337658719487502));
#4738=CARTESIAN_POINT('Ctrl Pts',(11.4174582184671,-26.234545724394,-0.759362367255897));
#4739=CARTESIAN_POINT('Ctrl Pts',(11.3060105618214,-26.5463258886116,-1.10586550012264));
#4740=CARTESIAN_POINT('Ctrl Pts',(11.1945629051758,-26.8581060528292,-1.45236863298939));
#4741=CARTESIAN_POINT('Ctrl Pts',(10.9745624584517,-27.2325591996199,-1.65504205590818));
#4742=CARTESIAN_POINT('Ctrl Pts',(10.7545620117277,-27.6070123464106,-1.85771547882697));
#4743=CARTESIAN_POINT('Ctrl Pts',(10.4908035184054,-28.0067292131839,-1.87641723476232));
#4744=CARTESIAN_POINT('Ctrl Pts',(10.227045025083,-28.4064460799573,-1.89511899069768));
#4745=CARTESIAN_POINT('Ctrl Pts',(9.99299004642868,-28.7890136145413,-1.72614496752462));
#4746=CARTESIAN_POINT('Ctrl Pts',(9.75893506777431,-29.1715811491253,-1.55717094435156));
#4747=CARTESIAN_POINT('Ctrl Pts',(9.62216201968436,-29.4979829349106,-1.2339885196899));
#4748=CARTESIAN_POINT('Ctrl Pts',(9.48538897159441,-29.8243847206959,-0.910806095028249));
#4749=CARTESIAN_POINT('Ctrl Pts',(9.4942083905325,-30.0667286564506,-0.497425511654571));
#4750=CARTESIAN_POINT('Ctrl Pts',(9.5030278094706,-30.3090725922053,-0.0840449282808927));
#4751=CARTESIAN_POINT('Ctrl Pts',(9.67691385823102,-30.4561152647978,0.337658719487502));
#4752=CARTESIAN_POINT('Ctrl Pts',(9.85079990699145,-30.6031579373903,0.759362367255897));
#4753=CARTESIAN_POINT('Ctrl Pts',(10.1765332779228,-30.6625315176518,1.10586550012264));
#4754=CARTESIAN_POINT('Ctrl Pts',(10.5022666488542,-30.7219050979132,1.45236863298939));
#4755=CARTESIAN_POINT('Ctrl Pts',(10.936552809864,-30.7186056956016,1.65504205590818));
#4756=CARTESIAN_POINT('Ctrl Pts',(11.3708389708737,-30.71530629329,1.85771547882697));
#4757=CARTESIAN_POINT('Ctrl Pts',(11.8488831784818,-30.6867431709956,1.87641723476232));
#4758=CARTESIAN_POINT('Ctrl Pts',(12.3269273860898,-30.6581800487013,1.89511899069768));
#4759=CARTESIAN_POINT('Ctrl Pts',(12.7752680790299,-30.6467662585964,1.72614496752462));
#4760=CARTESIAN_POINT('Ctrl Pts',(13.2236087719699,-30.6353524684915,1.55717094435156));
#4761=CARTESIAN_POINT('Ctrl Pts',(13.5746675343456,-30.6801044271852,1.2339885196899));
#4762=CARTESIAN_POINT('Ctrl Pts',(13.9257262967213,-30.7248563858789,0.910806095028249));
#4763=CARTESIAN_POINT('Ctrl Pts',(14.1311925920689,-30.8536661946033,0.497425511654571));
#4764=CARTESIAN_POINT('Ctrl Pts',(14.3366588874165,-30.9824760033276,0.084044928280893));
#4765=CARTESIAN_POINT('Ctrl Pts',(14.3770585529418,-31.2065870752141,-0.337658719487502));
#4766=CARTESIAN_POINT('Ctrl Pts',(14.4174582184671,-31.4306981471006,-0.759362367255897));
#4767=CARTESIAN_POINT('Ctrl Pts',(14.3060105618214,-31.7424783113183,-1.10586550012264));
#4768=CARTESIAN_POINT('Ctrl Pts',(14.1945629051758,-32.0542584755359,-1.45236863298939));
#4769=CARTESIAN_POINT('Ctrl Pts',(13.9745624584517,-32.4287116223265,-1.65504205590818));
#4770=CARTESIAN_POINT('Ctrl Pts',(13.7545620117276,-32.8031647691172,-1.85771547882697));
#4771=CARTESIAN_POINT('Ctrl Pts',(13.4908035184053,-33.2028816358906,-1.87641723476232));
#4772=CARTESIAN_POINT('Ctrl Pts',(13.227045025083,-33.602598502664,-1.89511899069768));
#4773=CARTESIAN_POINT('Ctrl Pts',(12.9929900464286,-33.9851660372479,-1.72614496752462));
#4774=CARTESIAN_POINT('Ctrl Pts',(12.7589350677743,-34.3677335718319,-1.55717094435156));
#4775=CARTESIAN_POINT('Ctrl Pts',(12.6221620196843,-34.6941353576172,-1.2339885196899));
#4776=CARTESIAN_POINT('Ctrl Pts',(12.4853889715944,-35.0205371434025,-0.910806095028249));
#4777=CARTESIAN_POINT('Ctrl Pts',(12.4942083905325,-35.2628810791572,-0.497425511654571));
#4778=CARTESIAN_POINT('Ctrl Pts',(12.5030278094706,-35.5052250149119,-0.0840449282808927));
#4779=CARTESIAN_POINT('Ctrl Pts',(12.676913858231,-35.6522676875044,0.337658719487502));
#4780=CARTESIAN_POINT('Ctrl Pts',(12.8507999069914,-35.799310360097,0.759362367255897));
#4781=CARTESIAN_POINT('Ctrl Pts',(13.1765332779228,-35.8586839403584,1.10586550012264));
#4782=CARTESIAN_POINT('Ctrl Pts',(13.5022666488542,-35.9180575206199,1.45236863298939));
#4783=CARTESIAN_POINT('Ctrl Pts',(13.9365528098639,-35.9147581183082,1.65504205590818));
#4784=CARTESIAN_POINT('Ctrl Pts',(14.3708389708737,-35.9114587159966,1.85771547882697));
#4785=CARTESIAN_POINT('Ctrl Pts',(14.8488831784817,-35.8828955937023,1.87641723476232));
#4786=CARTESIAN_POINT('Ctrl Pts',(15.3269273860897,-35.8543324714079,1.89511899069768));
#4787=CARTESIAN_POINT('Ctrl Pts',(15.7752680790298,-35.842918681303,1.72614496752462));
#4788=CARTESIAN_POINT('Ctrl Pts',(16.2236087719699,-35.8315048911981,1.55717094435156));
#4789=CARTESIAN_POINT('Ctrl Pts',(16.5746675343456,-35.8762568498918,1.2339885196899));
#4790=CARTESIAN_POINT('Ctrl Pts',(16.9257262967212,-35.9210088085856,0.910806095028249));
#4791=CARTESIAN_POINT('Ctrl Pts',(17.1311925920688,-36.0498186173099,0.497425511654571));
#4792=CARTESIAN_POINT('Ctrl Pts',(17.3366588874165,-36.1786284260343,0.084044928280893));
#4793=CARTESIAN_POINT('Ctrl Pts',(17.3770585529417,-36.4027394979208,-0.337658719487502));
#4794=CARTESIAN_POINT('Ctrl Pts',(17.417458218467,-36.6268505698073,-0.759362367255897));
#4795=CARTESIAN_POINT('Ctrl Pts',(17.3060105618214,-36.9386307340249,-1.10586550012264));
#4796=CARTESIAN_POINT('Ctrl Pts',(17.1945629051757,-37.2504108982425,-1.45236863298939));
#4797=CARTESIAN_POINT('Ctrl Pts',(16.9745624584517,-37.6248640450332,-1.65504205590818));
#4798=CARTESIAN_POINT('Ctrl Pts',(16.7545620117276,-37.9993171918239,-1.85771547882697));
#4799=CARTESIAN_POINT('Ctrl Pts',(16.4908035184053,-38.3990340585972,-1.87641723476232));
#4800=CARTESIAN_POINT('Ctrl Pts',(16.227045025083,-38.7987509253706,-1.89511899069768));
#4801=CARTESIAN_POINT('Ctrl Pts',(15.9929900464286,-39.1813184599546,-1.72614496752462));
#4802=CARTESIAN_POINT('Ctrl Pts',(15.7589350677742,-39.5638859945386,-1.55717094435156));
#4803=CARTESIAN_POINT('Ctrl Pts',(15.6221620196843,-39.8902877803239,-1.2339885196899));
#4804=CARTESIAN_POINT('Ctrl Pts',(15.4853889715943,-40.2166895661092,-0.910806095028249));
#4805=CARTESIAN_POINT('Ctrl Pts',(15.4942083905324,-40.4590335018639,-0.497425511654571));
#4806=CARTESIAN_POINT('Ctrl Pts',(15.5030278094705,-40.7013774376186,-0.0840449282808927));
#4807=CARTESIAN_POINT('Ctrl Pts',(15.676913858231,-40.8484201102111,0.337658719487502));
#4808=CARTESIAN_POINT('Ctrl Pts',(15.8507999069914,-40.9954627828037,0.759362367255897));
#4809=CARTESIAN_POINT('Ctrl Pts',(16.1765332779228,-41.0548363630651,1.10586550012264));
#4810=CARTESIAN_POINT('Ctrl Pts',(16.5022666488541,-41.1142099433265,1.45236863298939));
#4811=CARTESIAN_POINT('Ctrl Pts',(16.9365528098639,-41.1109105410149,1.65504205590818));
#4812=CARTESIAN_POINT('Ctrl Pts',(17.3708389708737,-41.1076111387033,1.85771547882697));
#4813=CARTESIAN_POINT('Ctrl Pts',(17.8488831784817,-41.0790480164089,1.87641723476232));
#4814=CARTESIAN_POINT('Ctrl Pts',(18.3269273860897,-41.0504848941146,1.89511899069768));
#4815=CARTESIAN_POINT('Ctrl Pts',(18.7752680790298,-41.0390711040097,1.72614496752462));
#4816=CARTESIAN_POINT('Ctrl Pts',(19.2236087719699,-41.0276573139048,1.55717094435156));
#4817=CARTESIAN_POINT('Ctrl Pts',(19.5746675343455,-41.0724092725985,1.2339885196899));
#4818=CARTESIAN_POINT('Ctrl Pts',(19.9257262967212,-41.1171612312922,0.910806095028249));
#4819=CARTESIAN_POINT('Ctrl Pts',(20.1311925920688,-41.2459710400166,0.497425511654571));
#4820=CARTESIAN_POINT('Ctrl Pts',(20.3366588874164,-41.374780848741,0.084044928280893));
#4821=CARTESIAN_POINT('Ctrl Pts',(20.3770585529417,-41.5988919206274,-0.337658719487502));
#4822=CARTESIAN_POINT('Ctrl Pts',(20.417458218467,-41.823002992514,-0.759362367255897));
#4823=CARTESIAN_POINT('Ctrl Pts',(20.3060105618213,-42.1347831567316,-1.10586550012264));
#4824=CARTESIAN_POINT('Ctrl Pts',(20.1945629051757,-42.4465633209492,-1.45236863298939));
#4825=CARTESIAN_POINT('Ctrl Pts',(19.9745624584516,-42.8210164677398,-1.65504205590818));
#4826=CARTESIAN_POINT('Ctrl Pts',(19.7545620117276,-43.1954696145305,-1.85771547882697));
#4827=CARTESIAN_POINT('Ctrl Pts',(19.4908035184053,-43.5951864813039,-1.87641723476232));
#4828=CARTESIAN_POINT('Ctrl Pts',(19.227045025083,-43.9949033480773,-1.89511899069768));
#4829=CARTESIAN_POINT('Ctrl Pts',(18.9929900464286,-44.3774708826612,-1.72614496752462));
#4830=CARTESIAN_POINT('Ctrl Pts',(18.7589350677742,-44.7600384172452,-1.55717094435156));
#4831=CARTESIAN_POINT('Ctrl Pts',(18.6221620196843,-45.0864402030305,-1.2339885196899));
#4832=CARTESIAN_POINT('Ctrl Pts',(2.69247988514806,-18.842665792852,-1.4918948215464));
#4833=CARTESIAN_POINT('Ctrl Pts',(2.50472787892454,-19.1985002938387,-1.01496252607126));
#4834=CARTESIAN_POINT('Ctrl Pts',(2.52538902495489,-19.434007405269,-0.437517342602656));
#4835=CARTESIAN_POINT('Ctrl Pts',(2.54605017098523,-19.6695145166993,0.139927840865946));
#4836=CARTESIAN_POINT('Ctrl Pts',(2.79225323278385,-19.7748049423473,0.703515811841622));
#4837=CARTESIAN_POINT('Ctrl Pts',(3.03845629458247,-19.8800953679953,1.2671037828173));
#4838=CARTESIAN_POINT('Ctrl Pts',(3.48265869315581,-19.871070823257,1.70520903169545));
#4839=CARTESIAN_POINT('Ctrl Pts',(3.92686109172914,-19.8620462785187,2.1433142805736));
#4840=CARTESIAN_POINT('Ctrl Pts',(4.50230405113288,-19.7772499606563,2.36916468980564));
#4841=CARTESIAN_POINT('Ctrl Pts',(5.07774701053662,-19.692453642794,2.59501509903768));
#4842=CARTESIAN_POINT('Ctrl Pts',(5.69167795219416,-19.5854362780169,2.5638782252017));
#4843=CARTESIAN_POINT('Ctrl Pts',(6.30560889385169,-19.4784189132398,2.53274135136572));
#4844=CARTESIAN_POINT('Ctrl Pts',(6.85765222227691,-19.4071323786218,2.25078423419363));
#4845=CARTESIAN_POINT('Ctrl Pts',(7.40969555070213,-19.3358458440039,1.96882711702155));
#4846=CARTESIAN_POINT('Ctrl Pts',(7.81173327121136,-19.3511650874962,1.4918948215464));
#4847=CARTESIAN_POINT('Ctrl Pts',(8.21377099172059,-19.3664843309885,1.01496252607126));
#4848=CARTESIAN_POINT('Ctrl Pts',(8.40739555997595,-19.5021309640373,0.437517342602656));
#4849=CARTESIAN_POINT('Ctrl Pts',(8.60102012823132,-19.637777597086,-0.139927840865945));
#4850=CARTESIAN_POINT('Ctrl Pts',(8.56910278071841,-19.9036409159171,-0.703515811841622));
#4851=CARTESIAN_POINT('Ctrl Pts',(8.5371854332055,-20.1695042347482,-1.2671037828173));
#4852=CARTESIAN_POINT('Ctrl Pts',(8.30726874891788,-20.5496825239655,-1.70520903169545));
#4853=CARTESIAN_POINT('Ctrl Pts',(8.07735206463027,-20.9298608131829,-2.1433142805736));
#4854=CARTESIAN_POINT('Ctrl Pts',(7.71619481951224,-21.3858108755242,-2.36916468980564));
#4855=CARTESIAN_POINT('Ctrl Pts',(7.35503757439421,-21.8417609378656,-2.59501509903768));
#4856=CARTESIAN_POINT('Ctrl Pts',(6.95539234702238,-22.3199320471218,-2.5638782252017));
#4857=CARTESIAN_POINT('Ctrl Pts',(6.55574711965056,-22.7981031563779,-2.53274135136572));
#4858=CARTESIAN_POINT('Ctrl Pts',(6.21798950551105,-23.2405434354749,-2.25078423419363));
#4859=CARTESIAN_POINT('Ctrl Pts',(5.88023189137154,-23.6829837145719,-1.96882711702155));
#4860=CARTESIAN_POINT('Ctrl Pts',(5.69247988514803,-24.0388182155586,-1.4918948215464));
#4861=CARTESIAN_POINT('Ctrl Pts',(5.50472787892451,-24.3946527165454,-1.01496252607126));
#4862=CARTESIAN_POINT('Ctrl Pts',(5.52538902495486,-24.6301598279757,-0.437517342602656));
#4863=CARTESIAN_POINT('Ctrl Pts',(5.5460501709852,-24.865666939406,0.139927840865946));
#4864=CARTESIAN_POINT('Ctrl Pts',(5.79225323278382,-24.970957365054,0.703515811841622));
#4865=CARTESIAN_POINT('Ctrl Pts',(6.03845629458244,-25.0762477907019,1.2671037828173));
#4866=CARTESIAN_POINT('Ctrl Pts',(6.48265869315577,-25.0672232459636,1.70520903169545));
#4867=CARTESIAN_POINT('Ctrl Pts',(6.92686109172911,-25.0581987012253,2.1433142805736));
#4868=CARTESIAN_POINT('Ctrl Pts',(7.50230405113285,-24.973402383363,2.36916468980564));
#4869=CARTESIAN_POINT('Ctrl Pts',(8.07774701053659,-24.8886060655007,2.59501509903768));
#4870=CARTESIAN_POINT('Ctrl Pts',(8.69167795219413,-24.7815887007236,2.5638782252017));
#4871=CARTESIAN_POINT('Ctrl Pts',(9.30560889385166,-24.6745713359464,2.53274135136572));
#4872=CARTESIAN_POINT('Ctrl Pts',(9.85765222227688,-24.6032848013285,2.25078423419363));
#4873=CARTESIAN_POINT('Ctrl Pts',(10.4096955507021,-24.5319982667106,1.96882711702155));
#4874=CARTESIAN_POINT('Ctrl Pts',(10.8117332712113,-24.5473175102029,1.4918948215464));
#4875=CARTESIAN_POINT('Ctrl Pts',(11.2137709917206,-24.5626367536952,1.01496252607126));
#4876=CARTESIAN_POINT('Ctrl Pts',(11.4073955599759,-24.6982833867439,0.437517342602656));
#4877=CARTESIAN_POINT('Ctrl Pts',(11.6010201282313,-24.8339300197927,-0.139927840865945));
#4878=CARTESIAN_POINT('Ctrl Pts',(11.5691027807184,-25.0997933386238,-0.703515811841622));
#4879=CARTESIAN_POINT('Ctrl Pts',(11.5371854332055,-25.3656566574548,-1.2671037828173));
#4880=CARTESIAN_POINT('Ctrl Pts',(11.3072687489179,-25.7458349466722,-1.70520903169545));
#4881=CARTESIAN_POINT('Ctrl Pts',(11.0773520646302,-26.1260132358895,-2.1433142805736));
#4882=CARTESIAN_POINT('Ctrl Pts',(10.7161948195122,-26.5819632982309,-2.36916468980564));
#4883=CARTESIAN_POINT('Ctrl Pts',(10.3550375743942,-27.0379133605723,-2.59501509903768));
#4884=CARTESIAN_POINT('Ctrl Pts',(9.95539234702235,-27.5160844698284,-2.5638782252017));
#4885=CARTESIAN_POINT('Ctrl Pts',(9.55574711965053,-27.9942555790846,-2.53274135136572));
#4886=CARTESIAN_POINT('Ctrl Pts',(9.21798950551102,-28.4366958581816,-2.25078423419363));
#4887=CARTESIAN_POINT('Ctrl Pts',(8.88023189137151,-28.8791361372786,-1.96882711702155));
#4888=CARTESIAN_POINT('Ctrl Pts',(8.692479885148,-29.2349706382653,-1.4918948215464));
#4889=CARTESIAN_POINT('Ctrl Pts',(8.50472787892448,-29.590805139252,-1.01496252607126));
#4890=CARTESIAN_POINT('Ctrl Pts',(8.52538902495483,-29.8263122506823,-0.437517342602656));
#4891=CARTESIAN_POINT('Ctrl Pts',(8.54605017098517,-30.0618193621126,0.139927840865946));
#4892=CARTESIAN_POINT('Ctrl Pts',(8.79225323278379,-30.1671097877606,0.703515811841622));
#4893=CARTESIAN_POINT('Ctrl Pts',(9.03845629458241,-30.2724002134086,1.2671037828173));
#4894=CARTESIAN_POINT('Ctrl Pts',(9.48265869315574,-30.2633756686703,1.70520903169545));
#4895=CARTESIAN_POINT('Ctrl Pts',(9.92686109172908,-30.254351123932,2.1433142805736));
#4896=CARTESIAN_POINT('Ctrl Pts',(10.5023040511328,-30.1695548060697,2.36916468980564));
#4897=CARTESIAN_POINT('Ctrl Pts',(11.0777470105366,-30.0847584882073,2.59501509903768));
#4898=CARTESIAN_POINT('Ctrl Pts',(11.6916779521941,-29.9777411234302,2.5638782252017));
#4899=CARTESIAN_POINT('Ctrl Pts',(12.3056088938516,-29.8707237586531,2.53274135136572));
#4900=CARTESIAN_POINT('Ctrl Pts',(12.8576522222768,-29.7994372240352,2.25078423419363));
#4901=CARTESIAN_POINT('Ctrl Pts',(13.4096955507021,-29.7281506894172,1.96882711702155));
#4902=CARTESIAN_POINT('Ctrl Pts',(13.8117332712113,-29.7434699329095,1.4918948215464));
#4903=CARTESIAN_POINT('Ctrl Pts',(14.2137709917205,-29.7587891764018,1.01496252607126));
#4904=CARTESIAN_POINT('Ctrl Pts',(14.4073955599759,-29.8944358094506,0.437517342602656));
#4905=CARTESIAN_POINT('Ctrl Pts',(14.6010201282313,-30.0300824424993,-0.139927840865945));
#4906=CARTESIAN_POINT('Ctrl Pts',(14.5691027807183,-30.2959457613304,-0.703515811841622));
#4907=CARTESIAN_POINT('Ctrl Pts',(14.5371854332054,-30.5618090801615,-1.2671037828173));
#4908=CARTESIAN_POINT('Ctrl Pts',(14.3072687489178,-30.9419873693788,-1.70520903169545));
#4909=CARTESIAN_POINT('Ctrl Pts',(14.0773520646302,-31.3221656585962,-2.1433142805736));
#4910=CARTESIAN_POINT('Ctrl Pts',(13.7161948195122,-31.7781157209375,-2.36916468980564));
#4911=CARTESIAN_POINT('Ctrl Pts',(13.3550375743941,-32.2340657832789,-2.59501509903768));
#4912=CARTESIAN_POINT('Ctrl Pts',(12.9553923470223,-32.7122368925351,-2.5638782252017));
#4913=CARTESIAN_POINT('Ctrl Pts',(12.5557471196505,-33.1904080017912,-2.53274135136572));
#4914=CARTESIAN_POINT('Ctrl Pts',(12.217989505511,-33.6328482808882,-2.25078423419363));
#4915=CARTESIAN_POINT('Ctrl Pts',(11.8802318913715,-34.0752885599852,-1.96882711702155));
#4916=CARTESIAN_POINT('Ctrl Pts',(11.692479885148,-34.4311230609719,-1.4918948215464));
#4917=CARTESIAN_POINT('Ctrl Pts',(11.5047278789244,-34.7869575619587,-1.01496252607126));
#4918=CARTESIAN_POINT('Ctrl Pts',(11.5253890249548,-35.022464673389,-0.437517342602656));
#4919=CARTESIAN_POINT('Ctrl Pts',(11.5460501709851,-35.2579717848193,0.139927840865946));
#4920=CARTESIAN_POINT('Ctrl Pts',(11.7922532327838,-35.3632622104672,0.703515811841622));
#4921=CARTESIAN_POINT('Ctrl Pts',(12.0384562945824,-35.4685526361152,1.2671037828173));
#4922=CARTESIAN_POINT('Ctrl Pts',(12.4826586931557,-35.4595280913769,1.70520903169545));
#4923=CARTESIAN_POINT('Ctrl Pts',(12.926861091729,-35.4505035466386,2.1433142805736));
#4924=CARTESIAN_POINT('Ctrl Pts',(13.5023040511328,-35.3657072287763,2.36916468980564));
#4925=CARTESIAN_POINT('Ctrl Pts',(14.0777470105365,-35.280910910914,2.59501509903768));
#4926=CARTESIAN_POINT('Ctrl Pts',(14.6916779521941,-35.1738935461369,2.5638782252017));
#4927=CARTESIAN_POINT('Ctrl Pts',(15.3056088938516,-35.0668761813597,2.53274135136572));
#4928=CARTESIAN_POINT('Ctrl Pts',(15.8576522222768,-34.9955896467418,2.25078423419363));
#4929=CARTESIAN_POINT('Ctrl Pts',(16.409695550702,-34.9243031121239,1.96882711702155));
#4930=CARTESIAN_POINT('Ctrl Pts',(16.8117332712113,-34.9396223556162,1.4918948215464));
#4931=CARTESIAN_POINT('Ctrl Pts',(17.2137709917205,-34.9549415991085,1.01496252607126));
#4932=CARTESIAN_POINT('Ctrl Pts',(17.4073955599759,-35.0905882321572,0.437517342602656));
#4933=CARTESIAN_POINT('Ctrl Pts',(17.6010201282312,-35.226234865206,-0.139927840865945));
#4934=CARTESIAN_POINT('Ctrl Pts',(17.5691027807183,-35.4920981840371,-0.703515811841622));
#4935=CARTESIAN_POINT('Ctrl Pts',(17.5371854332054,-35.7579615028681,-1.2671037828173));
#4936=CARTESIAN_POINT('Ctrl Pts',(17.3072687489178,-36.1381397920855,-1.70520903169545));
#4937=CARTESIAN_POINT('Ctrl Pts',(17.0773520646302,-36.5183180813028,-2.1433142805736));
#4938=CARTESIAN_POINT('Ctrl Pts',(16.7161948195121,-36.9742681436442,-2.36916468980564));
#4939=CARTESIAN_POINT('Ctrl Pts',(16.3550375743941,-37.4302182059856,-2.59501509903768));
#4940=CARTESIAN_POINT('Ctrl Pts',(15.9553923470223,-37.9083893152417,-2.5638782252017));
#4941=CARTESIAN_POINT('Ctrl Pts',(15.5557471196505,-38.3865604244979,-2.53274135136572));
#4942=CARTESIAN_POINT('Ctrl Pts',(15.217989505511,-38.8290007035949,-2.25078423419363));
#4943=CARTESIAN_POINT('Ctrl Pts',(14.8802318913715,-39.2714409826919,-1.96882711702155));
#4944=CARTESIAN_POINT('Ctrl Pts',(14.6924798851479,-39.6272754836786,-1.4918948215464));
#4945=CARTESIAN_POINT('Ctrl Pts',(14.5047278789244,-39.9831099846653,-1.01496252607126));
#4946=CARTESIAN_POINT('Ctrl Pts',(14.5253890249548,-40.2186170960956,-0.437517342602656));
#4947=CARTESIAN_POINT('Ctrl Pts',(14.5460501709851,-40.4541242075259,0.139927840865946));
#4948=CARTESIAN_POINT('Ctrl Pts',(14.7922532327837,-40.5594146331739,0.703515811841622));
#4949=CARTESIAN_POINT('Ctrl Pts',(15.0384562945823,-40.6647050588219,1.2671037828173));
#4950=CARTESIAN_POINT('Ctrl Pts',(15.4826586931557,-40.6556805140836,1.70520903169545));
#4951=CARTESIAN_POINT('Ctrl Pts',(15.926861091729,-40.6466559693453,2.1433142805736));
#4952=CARTESIAN_POINT('Ctrl Pts',(16.5023040511328,-40.5618596514829,2.36916468980564));
#4953=CARTESIAN_POINT('Ctrl Pts',(17.0777470105365,-40.4770633336206,2.59501509903768));
#4954=CARTESIAN_POINT('Ctrl Pts',(17.691677952194,-40.3700459688435,2.5638782252017));
#4955=CARTESIAN_POINT('Ctrl Pts',(18.3056088938516,-40.2630286040664,2.53274135136572));
#4956=CARTESIAN_POINT('Ctrl Pts',(18.8576522222768,-40.1917420694485,2.25078423419363));
#4957=CARTESIAN_POINT('Ctrl Pts',(19.409695550702,-40.1204555348305,1.96882711702155));
#4958=CARTESIAN_POINT('Ctrl Pts',(19.8117332712112,-40.1357747783228,1.4918948215464));
#4959=CARTESIAN_POINT('Ctrl Pts',(20.2137709917205,-40.1510940218152,1.01496252607126));
#4960=CARTESIAN_POINT('Ctrl Pts',(20.4073955599758,-40.2867406548639,0.437517342602656));
#4961=CARTESIAN_POINT('Ctrl Pts',(20.6010201282312,-40.4223872879126,-0.139927840865945));
#4962=CARTESIAN_POINT('Ctrl Pts',(20.5691027807183,-40.6882506067437,-0.703515811841622));
#4963=CARTESIAN_POINT('Ctrl Pts',(20.5371854332054,-40.9541139255748,-1.2671037828173));
#4964=CARTESIAN_POINT('Ctrl Pts',(20.3072687489178,-41.3342922147921,-1.70520903169545));
#4965=CARTESIAN_POINT('Ctrl Pts',(20.0773520646301,-41.7144705040095,-2.1433142805736));
#4966=CARTESIAN_POINT('Ctrl Pts',(19.7161948195121,-42.1704205663508,-2.36916468980564));
#4967=CARTESIAN_POINT('Ctrl Pts',(19.3550375743941,-42.6263706286922,-2.59501509903768));
#4968=CARTESIAN_POINT('Ctrl Pts',(18.9553923470223,-43.1045417379484,-2.5638782252017));
#4969=CARTESIAN_POINT('Ctrl Pts',(18.5557471196504,-43.5827128472045,-2.53274135136572));
#4970=CARTESIAN_POINT('Ctrl Pts',(18.2179895055109,-44.0251531263015,-2.25078423419363));
#4971=CARTESIAN_POINT('Ctrl Pts',(17.8802318913714,-44.4675934053985,-1.96882711702155));
#4972=CARTESIAN_POINT('Ctrl Pts',(17.6924798851479,-44.8234279063853,-1.4918948215464));
#4973=CARTESIAN_POINT('Ctrl Pts',(2.69247988514806,-19.542807947216,-2.20589829750609));
#4974=CARTESIAN_POINT('Ctrl Pts',(2.3635946338423,-19.9801257652426,-1.64906456309142));
#4975=CARTESIAN_POINT('Ctrl Pts',(2.28712243231041,-20.2717128410352,-0.928922098091803));
#4976=CARTESIAN_POINT('Ctrl Pts',(2.21065023077853,-20.5632999168279,-0.208779633092189));
#4977=CARTESIAN_POINT('Ctrl Pts',(2.42295829328197,-20.6881596294431,0.532038515331462));
#4978=CARTESIAN_POINT('Ctrl Pts',(2.63526635578541,-20.8130193420583,1.27285666375511));
#4979=CARTESIAN_POINT('Ctrl Pts',(3.1155254236359,-20.7831774696068,1.88762237576914));
#4980=CARTESIAN_POINT('Ctrl Pts',(3.5957844914864,-20.7533355971552,2.50238808778318));
#4981=CARTESIAN_POINT('Ctrl Pts',(4.27009432318328,-20.6114584639605,2.86933947451654));
#4982=CARTESIAN_POINT('Ctrl Pts',(4.94440415488017,-20.4695813307658,3.2362908612499));
#4983=CARTESIAN_POINT('Ctrl Pts',(5.70043037526654,-20.280525218564,3.28274870019663));
#4984=CARTESIAN_POINT('Ctrl Pts',(6.45645659565292,-20.0914691063622,3.32920653914337));
#4985=CARTESIAN_POINT('Ctrl Pts',(7.1656798966062,-19.929434672294,3.04596928553206));
#4986=CARTESIAN_POINT('Ctrl Pts',(7.87490319755949,-19.7674002382258,2.76273203192075));
#4987=CARTESIAN_POINT('Ctrl Pts',(8.41807416315096,-19.7012361646782,2.20589829750609));
#4988=CARTESIAN_POINT('Ctrl Pts',(8.96124512874244,-19.6350720911307,1.64906456309142));
#4989=CARTESIAN_POINT('Ctrl Pts',(9.25200304456004,-19.7146387598171,0.928922098091803));
#4990=CARTESIAN_POINT('Ctrl Pts',(9.54276096037763,-19.7942054285035,0.20877963309219));
#4991=CARTESIAN_POINT('Ctrl Pts',(9.5447386121599,-20.0404994603673,-0.532038515331461));
#4992=CARTESIAN_POINT('Ctrl Pts',(9.54671626394218,-20.2867934922312,-1.27285666375511));
#4993=CARTESIAN_POINT('Ctrl Pts',(9.28074291037739,-20.6877891091618,-1.88762237576914));
#4994=CARTESIAN_POINT('Ctrl Pts',(9.01476955681261,-21.0887847260924,-2.50238808778318));
#4995=CARTESIAN_POINT('Ctrl Pts',(8.55474543940143,-21.6018156037661,-2.86933947451654));
#4996=CARTESIAN_POINT('Ctrl Pts',(8.09472132199027,-22.1148464814399,-3.2362908612499));
#4997=CARTESIAN_POINT('Ctrl Pts',(7.5529808158896,-22.6750563381207,-3.28274870019663));
#4998=CARTESIAN_POINT('Ctrl Pts',(7.01124030978894,-23.2352661948015,-3.32920653914337));
#4999=CARTESIAN_POINT('Ctrl Pts',(6.51630272312137,-23.7684543733488,-3.04596928553206));
#5000=CARTESIAN_POINT('Ctrl Pts',(6.02136513645379,-24.3016425518961,-2.76273203192075));
#5001=CARTESIAN_POINT('Ctrl Pts',(5.69247988514803,-24.7389603699227,-2.20589829750609));
#5002=CARTESIAN_POINT('Ctrl Pts',(5.36359463384226,-25.1762781879492,-1.64906456309142));
#5003=CARTESIAN_POINT('Ctrl Pts',(5.28712243231038,-25.4678652637419,-0.928922098091803));
#5004=CARTESIAN_POINT('Ctrl Pts',(5.2106502307785,-25.7594523395345,-0.208779633092189));
#5005=CARTESIAN_POINT('Ctrl Pts',(5.42295829328193,-25.8843120521498,0.532038515331462));
#5006=CARTESIAN_POINT('Ctrl Pts',(5.63526635578538,-26.009171764765,1.27285666375511));
#5007=CARTESIAN_POINT('Ctrl Pts',(6.11552542363587,-25.9793298923134,1.88762237576914));
#5008=CARTESIAN_POINT('Ctrl Pts',(6.59578449148637,-25.9494880198619,2.50238808778318));
#5009=CARTESIAN_POINT('Ctrl Pts',(7.27009432318325,-25.8076108866672,2.86933947451654));
#5010=CARTESIAN_POINT('Ctrl Pts',(7.94440415488013,-25.6657337534725,3.2362908612499));
#5011=CARTESIAN_POINT('Ctrl Pts',(8.70043037526651,-25.4766776412707,3.28274870019663));
#5012=CARTESIAN_POINT('Ctrl Pts',(9.45645659565288,-25.2876215290689,3.32920653914337));
#5013=CARTESIAN_POINT('Ctrl Pts',(10.1656798966062,-25.1255870950007,3.04596928553206));
#5014=CARTESIAN_POINT('Ctrl Pts',(10.8749031975595,-24.9635526609324,2.76273203192075));
#5015=CARTESIAN_POINT('Ctrl Pts',(11.4180741631509,-24.8973885873849,2.20589829750609));
#5016=CARTESIAN_POINT('Ctrl Pts',(11.9612451287424,-24.8312245138374,1.64906456309142));
#5017=CARTESIAN_POINT('Ctrl Pts',(12.25200304456,-24.9107911825238,0.928922098091803));
#5018=CARTESIAN_POINT('Ctrl Pts',(12.5427609603776,-24.9903578512102,0.20877963309219));
#5019=CARTESIAN_POINT('Ctrl Pts',(12.5447386121599,-25.236651883074,-0.532038515331461));
#5020=CARTESIAN_POINT('Ctrl Pts',(12.5467162639421,-25.4829459149378,-1.27285666375511));
#5021=CARTESIAN_POINT('Ctrl Pts',(12.2807429103774,-25.8839415318684,-1.88762237576914));
#5022=CARTESIAN_POINT('Ctrl Pts',(12.0147695568126,-26.284937148799,-2.50238808778318));
#5023=CARTESIAN_POINT('Ctrl Pts',(11.5547454394014,-26.7979680264728,-2.86933947451654));
#5024=CARTESIAN_POINT('Ctrl Pts',(11.0947213219902,-27.3109989041465,-3.2362908612499));
#5025=CARTESIAN_POINT('Ctrl Pts',(10.5529808158896,-27.8712087608274,-3.28274870019663));
#5026=CARTESIAN_POINT('Ctrl Pts',(10.0112403097889,-28.4314186175082,-3.32920653914337));
#5027=CARTESIAN_POINT('Ctrl Pts',(9.51630272312133,-28.9646067960555,-3.04596928553206));
#5028=CARTESIAN_POINT('Ctrl Pts',(9.02136513645376,-29.4977949746027,-2.76273203192075));
#5029=CARTESIAN_POINT('Ctrl Pts',(8.692479885148,-29.9351127926293,-2.20589829750609));
#5030=CARTESIAN_POINT('Ctrl Pts',(8.36359463384224,-30.3724306106559,-1.64906456309142));
#5031=CARTESIAN_POINT('Ctrl Pts',(8.28712243231035,-30.6640176864485,-0.928922098091803));
#5032=CARTESIAN_POINT('Ctrl Pts',(8.21065023077846,-30.9556047622412,-0.208779633092189));
#5033=CARTESIAN_POINT('Ctrl Pts',(8.4229582932819,-31.0804644748564,0.532038515331462));
#5034=CARTESIAN_POINT('Ctrl Pts',(8.63526635578534,-31.2053241874716,1.27285666375511));
#5035=CARTESIAN_POINT('Ctrl Pts',(9.11552542363584,-31.1754823150201,1.88762237576914));
#5036=CARTESIAN_POINT('Ctrl Pts',(9.59578449148634,-31.1456404425685,2.50238808778318));
#5037=CARTESIAN_POINT('Ctrl Pts',(10.2700943231832,-31.0037633093738,2.86933947451654));
#5038=CARTESIAN_POINT('Ctrl Pts',(10.9444041548801,-30.8618861761791,3.2362908612499));
#5039=CARTESIAN_POINT('Ctrl Pts',(11.7004303752665,-30.6728300639773,3.28274870019663));
#5040=CARTESIAN_POINT('Ctrl Pts',(12.4564565956529,-30.4837739517755,3.32920653914337));
#5041=CARTESIAN_POINT('Ctrl Pts',(13.1656798966061,-30.3217395177073,3.04596928553206));
#5042=CARTESIAN_POINT('Ctrl Pts',(13.8749031975594,-30.1597050836391,2.76273203192075));
#5043=CARTESIAN_POINT('Ctrl Pts',(14.4180741631509,-30.0935410100915,2.20589829750609));
#5044=CARTESIAN_POINT('Ctrl Pts',(14.9612451287424,-30.027376936544,1.64906456309142));
#5045=CARTESIAN_POINT('Ctrl Pts',(15.25200304456,-30.1069436052304,0.928922098091803));
#5046=CARTESIAN_POINT('Ctrl Pts',(15.5427609603776,-30.1865102739168,0.20877963309219));
#5047=CARTESIAN_POINT('Ctrl Pts',(15.5447386121598,-30.4328043057806,-0.532038515331461));
#5048=CARTESIAN_POINT('Ctrl Pts',(15.5467162639421,-30.6790983376445,-1.27285666375511));
#5049=CARTESIAN_POINT('Ctrl Pts',(15.2807429103773,-31.0800939545751,-1.88762237576914));
#5050=CARTESIAN_POINT('Ctrl Pts',(15.0147695568125,-31.4810895715057,-2.50238808778318));
#5051=CARTESIAN_POINT('Ctrl Pts',(14.5547454394014,-31.9941204491794,-2.86933947451654));
#5052=CARTESIAN_POINT('Ctrl Pts',(14.0947213219902,-32.5071513268532,-3.2362908612499));
#5053=CARTESIAN_POINT('Ctrl Pts',(13.5529808158895,-33.067361183534,-3.28274870019663));
#5054=CARTESIAN_POINT('Ctrl Pts',(13.0112403097889,-33.6275710402148,-3.32920653914337));
#5055=CARTESIAN_POINT('Ctrl Pts',(12.5163027231213,-34.1607592187621,-3.04596928553206));
#5056=CARTESIAN_POINT('Ctrl Pts',(12.0213651364537,-34.6939473973094,-2.76273203192075));
#5057=CARTESIAN_POINT('Ctrl Pts',(11.692479885148,-35.131265215336,-2.20589829750609));
#5058=CARTESIAN_POINT('Ctrl Pts',(11.3635946338422,-35.5685830333625,-1.64906456309142));
#5059=CARTESIAN_POINT('Ctrl Pts',(11.2871224323103,-35.8601701091552,-0.928922098091803));
#5060=CARTESIAN_POINT('Ctrl Pts',(11.2106502307784,-36.1517571849478,-0.208779633092189));
#5061=CARTESIAN_POINT('Ctrl Pts',(11.4229582932819,-36.2766168975631,0.532038515331462));
#5062=CARTESIAN_POINT('Ctrl Pts',(11.6352663557853,-36.4014766101783,1.27285666375511));
#5063=CARTESIAN_POINT('Ctrl Pts',(12.1155254236358,-36.3716347377267,1.88762237576914));
#5064=CARTESIAN_POINT('Ctrl Pts',(12.5957844914863,-36.3417928652752,2.50238808778318));
#5065=CARTESIAN_POINT('Ctrl Pts',(13.2700943231832,-36.1999157320805,2.86933947451654));
#5066=CARTESIAN_POINT('Ctrl Pts',(13.9444041548801,-36.0580385988858,3.2362908612499));
#5067=CARTESIAN_POINT('Ctrl Pts',(14.7004303752664,-35.868982486684,3.28274870019663));
#5068=CARTESIAN_POINT('Ctrl Pts',(15.4564565956528,-35.6799263744822,3.32920653914337));
#5069=CARTESIAN_POINT('Ctrl Pts',(16.1656798966061,-35.517891940414,3.04596928553206));
#5070=CARTESIAN_POINT('Ctrl Pts',(16.8749031975594,-35.3558575063457,2.76273203192075));
#5071=CARTESIAN_POINT('Ctrl Pts',(17.4180741631509,-35.2896934327982,2.20589829750609));
#5072=CARTESIAN_POINT('Ctrl Pts',(17.9612451287423,-35.2235293592507,1.64906456309142));
#5073=CARTESIAN_POINT('Ctrl Pts',(18.2520030445599,-35.3030960279371,0.928922098091803));
#5074=CARTESIAN_POINT('Ctrl Pts',(18.5427609603775,-35.3826626966235,0.20877963309219));
#5075=CARTESIAN_POINT('Ctrl Pts',(18.5447386121598,-35.6289567284873,-0.532038515331461));
#5076=CARTESIAN_POINT('Ctrl Pts',(18.5467162639421,-35.8752507603511,-1.27285666375511));
#5077=CARTESIAN_POINT('Ctrl Pts',(18.2807429103773,-36.2762463772817,-1.88762237576914));
#5078=CARTESIAN_POINT('Ctrl Pts',(18.0147695568125,-36.6772419942123,-2.50238808778318));
#5079=CARTESIAN_POINT('Ctrl Pts',(17.5547454394013,-37.1902728718861,-2.86933947451654));
#5080=CARTESIAN_POINT('Ctrl Pts',(17.0947213219902,-37.7033037495598,-3.2362908612499));
#5081=CARTESIAN_POINT('Ctrl Pts',(16.5529808158895,-38.2635136062407,-3.28274870019663));
#5082=CARTESIAN_POINT('Ctrl Pts',(16.0112403097889,-38.8237234629215,-3.32920653914337));
#5083=CARTESIAN_POINT('Ctrl Pts',(15.5163027231213,-39.3569116414688,-3.04596928553206));
#5084=CARTESIAN_POINT('Ctrl Pts',(15.0213651364537,-39.890099820016,-2.76273203192075));
#5085=CARTESIAN_POINT('Ctrl Pts',(14.6924798851479,-40.3274176380426,-2.20589829750609));
#5086=CARTESIAN_POINT('Ctrl Pts',(14.3635946338422,-40.7647354560692,-1.64906456309142));
#5087=CARTESIAN_POINT('Ctrl Pts',(14.2871224323103,-41.0563225318618,-0.928922098091803));
#5088=CARTESIAN_POINT('Ctrl Pts',(14.2106502307784,-41.3479096076545,-0.208779633092189));
#5089=CARTESIAN_POINT('Ctrl Pts',(14.4229582932818,-41.4727693202697,0.532038515331462));
#5090=CARTESIAN_POINT('Ctrl Pts',(14.6352663557853,-41.5976290328849,1.27285666375511));
#5091=CARTESIAN_POINT('Ctrl Pts',(15.1155254236358,-41.5677871604334,1.88762237576914));
#5092=CARTESIAN_POINT('Ctrl Pts',(15.5957844914863,-41.5379452879818,2.50238808778318));
#5093=CARTESIAN_POINT('Ctrl Pts',(16.2700943231832,-41.3960681547871,2.86933947451654));
#5094=CARTESIAN_POINT('Ctrl Pts',(16.94440415488,-41.2541910215924,3.2362908612499));
#5095=CARTESIAN_POINT('Ctrl Pts',(17.7004303752664,-41.0651349093906,3.28274870019663));
#5096=CARTESIAN_POINT('Ctrl Pts',(18.4564565956528,-40.8760787971888,3.32920653914337));
#5097=CARTESIAN_POINT('Ctrl Pts',(19.1656798966061,-40.7140443631206,3.04596928553206));
#5098=CARTESIAN_POINT('Ctrl Pts',(19.8749031975594,-40.5520099290524,2.76273203192075));
#5099=CARTESIAN_POINT('Ctrl Pts',(20.4180741631508,-40.4858458555049,2.20589829750609));
#5100=CARTESIAN_POINT('Ctrl Pts',(20.9612451287423,-40.4196817819573,1.64906456309142));
#5101=CARTESIAN_POINT('Ctrl Pts',(21.2520030445599,-40.4992484506437,0.928922098091803));
#5102=CARTESIAN_POINT('Ctrl Pts',(21.5427609603775,-40.5788151193301,0.20877963309219));
#5103=CARTESIAN_POINT('Ctrl Pts',(21.5447386121598,-40.8251091511939,-0.532038515331461));
#5104=CARTESIAN_POINT('Ctrl Pts',(21.546716263942,-41.0714031830578,-1.27285666375511));
#5105=CARTESIAN_POINT('Ctrl Pts',(21.2807429103773,-41.4723987999884,-1.88762237576914));
#5106=CARTESIAN_POINT('Ctrl Pts',(21.0147695568125,-41.873394416919,-2.50238808778318));
#5107=CARTESIAN_POINT('Ctrl Pts',(20.5547454394013,-42.3864252945927,-2.86933947451654));
#5108=CARTESIAN_POINT('Ctrl Pts',(20.0947213219901,-42.8994561722665,-3.2362908612499));
#5109=CARTESIAN_POINT('Ctrl Pts',(19.5529808158895,-43.4596660289473,-3.28274870019663));
#5110=CARTESIAN_POINT('Ctrl Pts',(19.0112403097888,-44.0198758856281,-3.32920653914337));
#5111=CARTESIAN_POINT('Ctrl Pts',(18.5163027231212,-44.5530640641754,-3.04596928553206));
#5112=CARTESIAN_POINT('Ctrl Pts',(18.0213651364537,-45.0862522427227,-2.76273203192075));
#5113=CARTESIAN_POINT('Ctrl Pts',(17.6924798851479,-45.5235700607493,-2.20589829750609));
#5114=CARTESIAN_POINT('Ctrl Pts',(3.62216201968442,-19.8058202438613,-1.94799199564959));
#5115=CARTESIAN_POINT('Ctrl Pts',(3.34425572651223,-20.2137053466864,-1.54490813204841));
#5116=CARTESIAN_POINT('Ctrl Pts',(3.25594179788809,-20.5121292468035,-0.988830267143717));
#5117=CARTESIAN_POINT('Ctrl Pts',(3.16762786926396,-20.8105531469205,-0.432752402239027));
#5118=CARTESIAN_POINT('Ctrl Pts',(3.3076189187292,-20.9771651064803,0.166181422977342));
#5119=CARTESIAN_POINT('Ctrl Pts',(3.44760996819445,-21.1437770660401,0.765115248193711));
#5120=CARTESIAN_POINT('Ctrl Pts',(3.80940000840298,-21.1823333185883,1.28827884419634));
#5121=CARTESIAN_POINT('Ctrl Pts',(4.17119004861151,-21.2208895711365,1.81144244019896));
#5122=CARTESIAN_POINT('Ctrl Pts',(4.70434308191443,-21.1605093534924,2.15521684061908));
#5123=CARTESIAN_POINT('Ctrl Pts',(5.23749611521735,-21.1001291358485,2.49899124103919));
#5124=CARTESIAN_POINT('Ctrl Pts',(5.8576356015542,-20.9895272661294,2.59528770975726));
#5125=CARTESIAN_POINT('Ctrl Pts',(6.47777508789106,-20.8789253964104,2.69158417847533));
#5126=CARTESIAN_POINT('Ctrl Pts',(7.08329575335921,-20.7767637068552,2.52133001886304));
#5127=CARTESIAN_POINT('Ctrl Pts',(7.68881641882736,-20.6746020173,2.35107585925076));
#5128=CARTESIAN_POINT('Ctrl Pts',(8.18100842628526,-20.6378706589539,1.94799199564959));
#5129=CARTESIAN_POINT('Ctrl Pts',(8.67320043374317,-20.6011393006078,1.54490813204841));
#5130=CARTESIAN_POINT('Ctrl Pts',(8.97580007665302,-20.6738691449698,0.988830267143717));
#5131=CARTESIAN_POINT('Ctrl Pts',(9.27839971956287,-20.7465989893318,0.432752402239027));
#5132=CARTESIAN_POINT('Ctrl Pts',(9.35269438438334,-20.9511407742511,-0.166181422977342));
#5133=CARTESIAN_POINT('Ctrl Pts',(9.4269890492038,-21.1556825591703,-0.765115248193711));
#5134=CARTESIAN_POINT('Ctrl Pts',(9.27948472328098,-21.4882800511012,-1.28827884419634));
#5135=CARTESIAN_POINT('Ctrl Pts',(9.13198039735816,-21.8208775430321,-1.81144244019896));
#5136=CARTESIAN_POINT('Ctrl Pts',(8.81311307834095,-22.2524115051551,-2.15521684061908));
#5137=CARTESIAN_POINT('Ctrl Pts',(8.49424575932375,-22.6839454672782,-2.49899124103919));
#5138=CARTESIAN_POINT('Ctrl Pts',(8.0883919872726,-23.1657010814762,-2.59528770975726));
#5139=CARTESIAN_POINT('Ctrl Pts',(7.68253821522146,-23.6474566956743,-2.69158417847533));
#5140=CARTESIAN_POINT('Ctrl Pts',(7.29130326403902,-24.1207721297085,-2.52133001886305));
#5141=CARTESIAN_POINT('Ctrl Pts',(6.90006831285659,-24.5940875637428,-2.35107585925076));
#5142=CARTESIAN_POINT('Ctrl Pts',(6.62216201968439,-25.0019726665679,-1.94799199564959));
#5143=CARTESIAN_POINT('Ctrl Pts',(6.34425572651219,-25.4098577693931,-1.54490813204841));
#5144=CARTESIAN_POINT('Ctrl Pts',(6.25594179788806,-25.7082816695101,-0.988830267143717));
#5145=CARTESIAN_POINT('Ctrl Pts',(6.16762786926392,-26.0067055696272,-0.432752402239027));
#5146=CARTESIAN_POINT('Ctrl Pts',(6.30761891872917,-26.1733175291869,0.166181422977342));
#5147=CARTESIAN_POINT('Ctrl Pts',(6.44760996819441,-26.3399294887468,0.765115248193711));
#5148=CARTESIAN_POINT('Ctrl Pts',(6.80940000840295,-26.3784857412949,1.28827884419634));
#5149=CARTESIAN_POINT('Ctrl Pts',(7.17119004861148,-26.4170419938431,1.81144244019896));
#5150=CARTESIAN_POINT('Ctrl Pts',(7.7043430819144,-26.3566617761991,2.15521684061908));
#5151=CARTESIAN_POINT('Ctrl Pts',(8.23749611521731,-26.2962815585551,2.49899124103919));
#5152=CARTESIAN_POINT('Ctrl Pts',(8.85763560155417,-26.1856796888361,2.59528770975726));
#5153=CARTESIAN_POINT('Ctrl Pts',(9.47777508789103,-26.0750778191171,2.69158417847533));
#5154=CARTESIAN_POINT('Ctrl Pts',(10.0832957533592,-25.9729161295619,2.52133001886304));
#5155=CARTESIAN_POINT('Ctrl Pts',(10.6888164188273,-25.8707544400067,2.35107585925076));
#5156=CARTESIAN_POINT('Ctrl Pts',(11.1810084262852,-25.8340230816606,1.94799199564959));
#5157=CARTESIAN_POINT('Ctrl Pts',(11.6732004337431,-25.7972917233145,1.54490813204841));
#5158=CARTESIAN_POINT('Ctrl Pts',(11.975800076653,-25.8700215676765,0.988830267143717));
#5159=CARTESIAN_POINT('Ctrl Pts',(12.2783997195628,-25.9427514120385,0.432752402239027));
#5160=CARTESIAN_POINT('Ctrl Pts',(12.3526943843833,-26.1472931969577,-0.166181422977342));
#5161=CARTESIAN_POINT('Ctrl Pts',(12.4269890492038,-26.351834981877,-0.765115248193711));
#5162=CARTESIAN_POINT('Ctrl Pts',(12.279484723281,-26.6844324738078,-1.28827884419634));
#5163=CARTESIAN_POINT('Ctrl Pts',(12.1319803973581,-27.0170299657387,-1.81144244019896));
#5164=CARTESIAN_POINT('Ctrl Pts',(11.8131130783409,-27.4485639278618,-2.15521684061908));
#5165=CARTESIAN_POINT('Ctrl Pts',(11.4942457593237,-27.8800978899848,-2.49899124103919));
#5166=CARTESIAN_POINT('Ctrl Pts',(11.0883919872726,-28.3618535041829,-2.59528770975726));
#5167=CARTESIAN_POINT('Ctrl Pts',(10.6825382152214,-28.8436091183809,-2.69158417847533));
#5168=CARTESIAN_POINT('Ctrl Pts',(10.291303264039,-29.3169245524152,-2.52133001886305));
#5169=CARTESIAN_POINT('Ctrl Pts',(9.90006831285655,-29.7902399864494,-2.35107585925076));
#5170=CARTESIAN_POINT('Ctrl Pts',(9.62216201968436,-30.1981250892746,-1.94799199564959));
#5171=CARTESIAN_POINT('Ctrl Pts',(9.34425572651217,-30.6060101920997,-1.54490813204841));
#5172=CARTESIAN_POINT('Ctrl Pts',(9.25594179788803,-30.9044340922168,-0.988830267143717));
#5173=CARTESIAN_POINT('Ctrl Pts',(9.16762786926389,-31.2028579923338,-0.432752402239027));
#5174=CARTESIAN_POINT('Ctrl Pts',(9.30761891872914,-31.3694699518936,0.166181422977342));
#5175=CARTESIAN_POINT('Ctrl Pts',(9.44760996819438,-31.5360819114534,0.765115248193711));
#5176=CARTESIAN_POINT('Ctrl Pts',(9.80940000840292,-31.5746381640016,1.28827884419634));
#5177=CARTESIAN_POINT('Ctrl Pts',(10.1711900486115,-31.6131944165497,1.81144244019896));
#5178=CARTESIAN_POINT('Ctrl Pts',(10.7043430819144,-31.5528141989058,2.15521684061908));
#5179=CARTESIAN_POINT('Ctrl Pts',(11.2374961152173,-31.4924339812617,2.49899124103919));
#5180=CARTESIAN_POINT('Ctrl Pts',(11.8576356015541,-31.3818321115427,2.59528770975726));
#5181=CARTESIAN_POINT('Ctrl Pts',(12.477775087891,-31.2712302418237,2.69158417847533));
#5182=CARTESIAN_POINT('Ctrl Pts',(13.0832957533591,-31.1690685522685,2.52133001886304));
#5183=CARTESIAN_POINT('Ctrl Pts',(13.6888164188273,-31.0669068627133,2.35107585925076));
#5184=CARTESIAN_POINT('Ctrl Pts',(14.1810084262852,-31.0301755043672,1.94799199564959));
#5185=CARTESIAN_POINT('Ctrl Pts',(14.6732004337431,-30.9934441460211,1.54490813204841));
#5186=CARTESIAN_POINT('Ctrl Pts',(14.975800076653,-31.0661739903831,0.988830267143717));
#5187=CARTESIAN_POINT('Ctrl Pts',(15.2783997195628,-31.1389038347451,0.432752402239027));
#5188=CARTESIAN_POINT('Ctrl Pts',(15.3526943843833,-31.3434456196644,-0.166181422977342));
#5189=CARTESIAN_POINT('Ctrl Pts',(15.4269890492037,-31.5479874045836,-0.765115248193711));
#5190=CARTESIAN_POINT('Ctrl Pts',(15.2794847232809,-31.8805848965145,-1.28827884419634));
#5191=CARTESIAN_POINT('Ctrl Pts',(15.1319803973581,-32.2131823884454,-1.81144244019896));
#5192=CARTESIAN_POINT('Ctrl Pts',(14.8131130783409,-32.6447163505684,-2.15521684061908));
#5193=CARTESIAN_POINT('Ctrl Pts',(14.4942457593237,-33.0762503126915,-2.49899124103919));
#5194=CARTESIAN_POINT('Ctrl Pts',(14.0883919872725,-33.5580059268895,-2.59528770975726));
#5195=CARTESIAN_POINT('Ctrl Pts',(13.6825382152214,-34.0397615410876,-2.69158417847533));
#5196=CARTESIAN_POINT('Ctrl Pts',(13.291303264039,-34.5130769751218,-2.52133001886305));
#5197=CARTESIAN_POINT('Ctrl Pts',(12.9000683128565,-34.9863924091561,-2.35107585925076));
#5198=CARTESIAN_POINT('Ctrl Pts',(12.6221620196843,-35.3942775119812,-1.94799199564959));
#5199=CARTESIAN_POINT('Ctrl Pts',(12.3442557265121,-35.8021626148064,-1.54490813204841));
#5200=CARTESIAN_POINT('Ctrl Pts',(12.255941797888,-36.1005865149234,-0.988830267143717));
#5201=CARTESIAN_POINT('Ctrl Pts',(12.1676278692639,-36.3990104150405,-0.432752402239027));
#5202=CARTESIAN_POINT('Ctrl Pts',(12.3076189187291,-36.5656223746002,0.166181422977342));
#5203=CARTESIAN_POINT('Ctrl Pts',(12.4476099681944,-36.73223433416,0.765115248193711));
#5204=CARTESIAN_POINT('Ctrl Pts',(12.8094000084029,-36.7707905867082,1.28827884419634));
#5205=CARTESIAN_POINT('Ctrl Pts',(13.1711900486114,-36.8093468392564,1.81144244019896));
#5206=CARTESIAN_POINT('Ctrl Pts',(13.7043430819143,-36.7489666216124,2.15521684061908));
#5207=CARTESIAN_POINT('Ctrl Pts',(14.2374961152173,-36.6885864039684,2.49899124103919));
#5208=CARTESIAN_POINT('Ctrl Pts',(14.8576356015541,-36.5779845342494,2.59528770975726));
#5209=CARTESIAN_POINT('Ctrl Pts',(15.477775087891,-36.4673826645304,2.69158417847533));
#5210=CARTESIAN_POINT('Ctrl Pts',(16.0832957533591,-36.3652209749752,2.52133001886304));
#5211=CARTESIAN_POINT('Ctrl Pts',(16.6888164188273,-36.26305928542,2.35107585925076));
#5212=CARTESIAN_POINT('Ctrl Pts',(17.1810084262852,-36.2263279270739,1.94799199564959));
#5213=CARTESIAN_POINT('Ctrl Pts',(17.6732004337431,-36.1895965687278,1.54490813204841));
#5214=CARTESIAN_POINT('Ctrl Pts',(17.9758000766529,-36.2623264130898,0.988830267143717));
#5215=CARTESIAN_POINT('Ctrl Pts',(18.2783997195628,-36.3350562574518,0.432752402239027));
#5216=CARTESIAN_POINT('Ctrl Pts',(18.3526943843832,-36.539598042371,-0.166181422977342));
#5217=CARTESIAN_POINT('Ctrl Pts',(18.4269890492037,-36.7441398272903,-0.765115248193711));
#5218=CARTESIAN_POINT('Ctrl Pts',(18.2794847232809,-37.0767373192211,-1.28827884419634));
#5219=CARTESIAN_POINT('Ctrl Pts',(18.1319803973581,-37.409334811152,-1.81144244019896));
#5220=CARTESIAN_POINT('Ctrl Pts',(17.8131130783409,-37.8408687732751,-2.15521684061908));
#5221=CARTESIAN_POINT('Ctrl Pts',(17.4942457593237,-38.2724027353981,-2.49899124103919));
#5222=CARTESIAN_POINT('Ctrl Pts',(17.0883919872725,-38.7541583495962,-2.59528770975726));
#5223=CARTESIAN_POINT('Ctrl Pts',(16.6825382152214,-39.2359139637942,-2.69158417847533));
#5224=CARTESIAN_POINT('Ctrl Pts',(16.2913032640389,-39.7092293978285,-2.52133001886305));
#5225=CARTESIAN_POINT('Ctrl Pts',(15.9000683128565,-40.1825448318627,-2.35107585925076));
#5226=CARTESIAN_POINT('Ctrl Pts',(15.6221620196843,-40.5904299346879,-1.94799199564959));
#5227=CARTESIAN_POINT('Ctrl Pts',(15.3442557265121,-40.998315037513,-1.54490813204841));
#5228=CARTESIAN_POINT('Ctrl Pts',(15.255941797888,-41.2967389376301,-0.988830267143717));
#5229=CARTESIAN_POINT('Ctrl Pts',(15.1676278692638,-41.5951628377471,-0.432752402239027));
#5230=CARTESIAN_POINT('Ctrl Pts',(15.3076189187291,-41.7617747973069,0.166181422977342));
#5231=CARTESIAN_POINT('Ctrl Pts',(15.4476099681943,-41.9283867568667,0.765115248193711));
#5232=CARTESIAN_POINT('Ctrl Pts',(15.8094000084029,-41.9669430094149,1.28827884419634));
#5233=CARTESIAN_POINT('Ctrl Pts',(16.1711900486114,-42.0054992619631,1.81144244019896));
#5234=CARTESIAN_POINT('Ctrl Pts',(16.7043430819143,-41.945119044319,2.15521684061908));
#5235=CARTESIAN_POINT('Ctrl Pts',(17.2374961152172,-41.884738826675,2.49899124103919));
#5236=CARTESIAN_POINT('Ctrl Pts',(17.8576356015541,-41.774136956956,2.59528770975726));
#5237=CARTESIAN_POINT('Ctrl Pts',(18.4777750878909,-41.6635350872371,2.69158417847533));
#5238=CARTESIAN_POINT('Ctrl Pts',(19.0832957533591,-41.5613733976818,2.52133001886304));
#5239=CARTESIAN_POINT('Ctrl Pts',(19.6888164188272,-41.4592117081266,2.35107585925076));
#5240=CARTESIAN_POINT('Ctrl Pts',(20.1810084262851,-41.4224803497805,1.94799199564959));
#5241=CARTESIAN_POINT('Ctrl Pts',(20.673200433743,-41.3857489914344,1.54490813204841));
#5242=CARTESIAN_POINT('Ctrl Pts',(20.9758000766529,-41.4584788357964,0.988830267143717));
#5243=CARTESIAN_POINT('Ctrl Pts',(21.2783997195627,-41.5312086801584,0.432752402239027));
#5244=CARTESIAN_POINT('Ctrl Pts',(21.3526943843832,-41.7357504650777,-0.166181422977342));
#5245=CARTESIAN_POINT('Ctrl Pts',(21.4269890492037,-41.940292249997,-0.765115248193711));
#5246=CARTESIAN_POINT('Ctrl Pts',(21.2794847232809,-42.2728897419278,-1.28827884419634));
#5247=CARTESIAN_POINT('Ctrl Pts',(21.131980397358,-42.6054872338587,-1.81144244019896));
#5248=CARTESIAN_POINT('Ctrl Pts',(20.8131130783408,-43.0370211959817,-2.15521684061908));
#5249=CARTESIAN_POINT('Ctrl Pts',(20.4942457593236,-43.4685551581048,-2.49899124103919));
#5250=CARTESIAN_POINT('Ctrl Pts',(20.0883919872725,-43.9503107723028,-2.59528770975726));
#5251=CARTESIAN_POINT('Ctrl Pts',(19.6825382152213,-44.4320663865008,-2.69158417847533));
#5252=CARTESIAN_POINT('Ctrl Pts',(19.2913032640389,-44.9053818205351,-2.52133001886305));
#5253=CARTESIAN_POINT('Ctrl Pts',(18.9000683128565,-45.3786972545694,-2.35107585925076));
#5254=CARTESIAN_POINT('Ctrl Pts',(18.6221620196843,-45.7865823573945,-1.94799199564959));
#5255=CARTESIAN_POINT('',(4.2032568854171,-20.2749544279031,1.13384235805382));
#5256=CARTESIAN_POINT('',(3.23546955922298,-20.8337067011995,-0.275782109461829));
#5257=CARTESIAN_POINT('Ctrl Pts',(4.20325688541709,-20.2749544279031,1.13384235805383));
#5258=CARTESIAN_POINT('Ctrl Pts',(4.17353067602025,-20.2921168629003,1.00157233741796));
#5259=CARTESIAN_POINT('Ctrl Pts',(4.1267106773264,-20.3191484017499,0.826930627992248));
#5260=CARTESIAN_POINT('Ctrl Pts',(3.98429110156123,-20.4013743821558,0.245673499496276));
#5261=CARTESIAN_POINT('Ctrl Pts',(3.95326965129557,-20.4192846248171,0.063434900146937));
#5262=CARTESIAN_POINT('Ctrl Pts',(3.87127320952701,-20.4666252925448,-0.303997345944323));
#5263=CARTESIAN_POINT('Ctrl Pts',(3.83289404529189,-20.4887835133472,-0.445928116938839));
#5264=CARTESIAN_POINT('Ctrl Pts',(3.76001379967537,-20.5308609427725,-0.580444950877261));
#5265=CARTESIAN_POINT('Ctrl Pts',(3.73627207202441,-20.5445682356228,-0.614841199081482));
#5266=CARTESIAN_POINT('Ctrl Pts',(3.68747821159276,-20.5727393840778,-0.658095559969579));
#5267=CARTESIAN_POINT('Ctrl Pts',(3.66574669183764,-20.5852860829322,-0.67126084025885));
#5268=CARTESIAN_POINT('Ctrl Pts',(3.62032504182814,-20.6115102847922,-0.685243879141505));
#5269=CARTESIAN_POINT('Ctrl Pts',(3.59837730297536,-20.6241818176628,-0.686792486479322));
#5270=CARTESIAN_POINT('Ctrl Pts',(3.55016879873963,-20.6520150105605,-0.68047811375245));
#5271=CARTESIAN_POINT('Ctrl Pts',(3.52485041998139,-20.6666325833848,-0.670963714902961));
#5272=CARTESIAN_POINT('Ctrl Pts',(3.46539099876758,-20.7009614962285,-0.637810386100254));
#5273=CARTESIAN_POINT('Ctrl Pts',(3.43258170225768,-20.7199039523579,-0.609116109766831));
#5274=CARTESIAN_POINT('Ctrl Pts',(3.36695703423207,-20.757792372108,-0.536557857713739));
#5275=CARTESIAN_POINT('Ctrl Pts',(3.33473510032454,-20.7763957143233,-0.488582718568797));
#5276=CARTESIAN_POINT('Ctrl Pts',(3.29324460446342,-20.8003502632775,-0.412780370862962));
#5277=CARTESIAN_POINT('Ctrl Pts',(3.28021410458973,-20.8078734258878,-0.38607598492762));
#5278=CARTESIAN_POINT('Ctrl Pts',(3.25633438200707,-20.8216603901491,-0.331726097207036));
#5279=CARTESIAN_POINT('Ctrl Pts',(3.24541906679483,-20.8279623503246,-0.303953413725008));
#5280=CARTESIAN_POINT('Ctrl Pts',(3.23546955922298,-20.8337067011995,-0.275782109461826));
#5281=CARTESIAN_POINT('',(18.798465077288,-44.7175311486928,-1.53746850370033));
#5282=CARTESIAN_POINT('Ctrl Pts',(4.2032568854171,-20.2749544279031,1.13384235805382));
#5283=CARTESIAN_POINT('Ctrl Pts',(4.24461700886028,-20.2820537271614,1.17645708943624));
#5284=CARTESIAN_POINT('Ctrl Pts',(4.28785838370013,-20.2884806648945,1.21788038932571));
#5285=CARTESIAN_POINT('Ctrl Pts',(4.33277900087509,-20.2941850472034,1.25785531692514));
#5286=CARTESIAN_POINT('Ctrl Pts',(4.37777282801695,-20.2998987263045,1.29789539418882));
#5287=CARTESIAN_POINT('Ctrl Pts',(4.42445090390001,-20.3048873562845,1.33648171343798));
#5288=CARTESIAN_POINT('Ctrl Pts',(4.4725682388037,-20.3091157007804,1.37338328451688));
#5289=CARTESIAN_POINT('Ctrl Pts',(4.5206565890512,-20.3133414982293,1.41026262702987));
#5290=CARTESIAN_POINT('Ctrl Pts',(4.57018182638758,-20.3168078525493,1.44545870665561));
#5291=CARTESIAN_POINT('Ctrl Pts',(4.62086588701489,-20.3194963391104,1.47877717452078));
#5292=CARTESIAN_POINT('Ctrl Pts',(4.67156701372341,-20.3221857309251,1.51210686121238));
#5293=CARTESIAN_POINT('Ctrl Pts',(4.72342700590654,-20.3240967190121,1.54355727141904));
#5294=CARTESIAN_POINT('Ctrl Pts',(4.77614434033978,-20.3252282718733,1.57297724251041));
#5295=CARTESIAN_POINT('Ctrl Pts',(4.82886167477302,-20.3263598247345,1.60239721360178));
#5296=CARTESIAN_POINT('Ctrl Pts',(4.88243556544018,-20.3267119951369,1.62978652591198));
#5297=CARTESIAN_POINT('Ctrl Pts',(4.93655280986403,-20.3263008501883,1.65504205590817));
#5298=CARTESIAN_POINT('Ctrl Pts',(4.99059318650869,-20.3258902892273,1.68026171311514));
#5299=CARTESIAN_POINT('Ctrl Pts',(5.04595605131711,-20.3251645199386,1.70359676647101));
#5300=CARTESIAN_POINT('Ctrl Pts',(5.10236312310759,-20.3241201576957,1.72487226661214));
#5301=CARTESIAN_POINT('Ctrl Pts',(5.15878989379679,-20.3230754307329,1.74615519674227));
#5302=CARTESIAN_POINT('Ctrl Pts',(5.21626093600896,-20.3217118741235,1.76537666733536));
#5303=CARTESIAN_POINT('Ctrl Pts',(5.27446758778795,-20.3200331541901,1.78240346403954));
#5304=CARTESIAN_POINT('Ctrl Pts',(5.33272590071357,-20.3183529443137,1.79944537282823));
#5305=CARTESIAN_POINT('Ctrl Pts',(5.3917203532243,-20.3163570229522,1.81428839412964));
#5306=CARTESIAN_POINT('Ctrl Pts',(5.4511221884305,-20.3140561535612,1.82684686809475));
#5307=CARTESIAN_POINT('Ctrl Pts',(5.51047877834456,-20.3117570367003,1.83939577649979));
#5308=CARTESIAN_POINT('Ctrl Pts',(5.57024130034645,-20.3091534753514,1.84966349840266));
#5309=CARTESIAN_POINT('Ctrl Pts',(5.6300746296415,-20.3062628967142,1.85761563656239));
#5310=CARTESIAN_POINT('Ctrl Pts',(5.68987388180331,-20.3033739643607,1.86556324570669));
#5311=CARTESIAN_POINT('Ctrl Pts',(5.74974304733144,-20.300198402808,1.87119797990082));
#5312=CARTESIAN_POINT('Ctrl Pts',(5.80935283862858,-20.2967595360185,1.87453687269572));
#5313=CARTESIAN_POINT('Ctrl Pts',(5.82254342932584,-20.2959985757249,1.8752757105155));
#5314=CARTESIAN_POINT('Ctrl Pts',(5.83572136684984,-20.2952247433012,1.87590232633985));
#5315=CARTESIAN_POINT('Ctrl Pts',(5.84888317848182,-20.2944383255823,1.87641723476232));
#5316=CARTESIAN_POINT('Ctrl Pts',(5.90836858545831,-20.2908840748935,1.87874438682333));
#5317=CARTESIAN_POINT('Ctrl Pts',(5.96835659021567,-20.2874879798102,1.87880825693467));
#5318=CARTESIAN_POINT('Ctrl Pts',(6.02852369732613,-20.2842727601632,1.87655505226089));
#5319=CARTESIAN_POINT('Ctrl Pts',(6.08871181644296,-20.2810564176731,1.87430106070614));
#5320=CARTESIAN_POINT('Ctrl Pts',(6.14907837120147,-20.2780211361157,1.86972820122922));
#5321=CARTESIAN_POINT('Ctrl Pts',(6.20928772635011,-20.2751861548528,1.86283322829492));
#5322=CARTESIAN_POINT('Ctrl Pts',(6.26955052013898,-20.2723486574104,1.8559321357472));
#5323=CARTESIAN_POINT('Ctrl Pts',(6.32965499818605,-20.2697118625066,1.84670481534537));
#5324=CARTESIAN_POINT('Ctrl Pts',(6.38926509597254,-20.2672907526587,1.83519995710464));
#5325=CARTESIAN_POINT('Ctrl Pts',(6.44882978983705,-20.264871486926,1.82370386190416));
#5326=CARTESIAN_POINT('Ctrl Pts',(6.50790004501559,-20.2626676060139,1.80993391118304));
#5327=CARTESIAN_POINT('Ctrl Pts',(6.56615344995033,-20.2606891971314,1.79398881938349));
#5328=CARTESIAN_POINT('Ctrl Pts',(6.624373677573,-20.2587119150207,1.7780528088606));
#5329=CARTESIAN_POINT('Ctrl Pts',(6.68177726190263,-20.2569598574367,1.75994451788707));
#5330=CARTESIAN_POINT('Ctrl Pts',(6.73806677323732,-20.2554379551772,1.73980808434991));
#5331=CARTESIAN_POINT('Ctrl Pts',(6.75052264480493,-20.255101185171,1.73535224836872));
#5332=CARTESIAN_POINT('Ctrl Pts',(6.76292408311165,-20.2547756647794,1.73079726584414));
#5333=CARTESIAN_POINT('Ctrl Pts',(6.77526807902992,-20.2544614131831,1.72614496752461));
#5334=CARTESIAN_POINT('Ctrl Pts',(6.8310573306498,-20.2530411387843,1.70511869343335));
#5335=CARTESIAN_POINT('Ctrl Pts',(6.88646819440133,-20.2522876572929,1.68189873004129));
#5336=CARTESIAN_POINT('Ctrl Pts',(6.94118196331999,-20.2522209239189,1.65656309537197));
#5337=CARTESIAN_POINT('Ctrl Pts',(6.99591483978929,-20.2521541672398,1.63121861280326));
#5338=CARTESIAN_POINT('Ctrl Pts',(7.04994933840857,-20.2527746999987,1.60375713415829));
#5339=CARTESIAN_POINT('Ctrl Pts',(7.10297435817382,-20.2540875967032,1.57430602553659));
#5340=CARTESIAN_POINT('Ctrl Pts',(7.1560464401433,-20.2554016586654,1.5448287776679));
#5341=CARTESIAN_POINT('Ctrl Pts',(7.20810648127216,-20.2574093215818,1.51335869953408));
#5342=CARTESIAN_POINT('Ctrl Pts',(7.25886231563989,-20.2601002231023,1.48006918735993));
#5343=CARTESIAN_POINT('Ctrl Pts',(7.30957949021628,-20.2627890750122,1.44680503119875));
#5344=CARTESIAN_POINT('Ctrl Pts',(7.35899377471803,-20.2661600713697,1.41172471547131));
#5345=CARTESIAN_POINT('Ctrl Pts',(7.40684422911068,-20.2701878087831,1.37504051469708));
#5346=CARTESIAN_POINT('Ctrl Pts',(7.45466743102822,-20.2742132522618,1.33837720683351));
#5347=CARTESIAN_POINT('Ctrl Pts',(7.50092805869645,-20.2788945837058,1.30011245980337));
#5348=CARTESIAN_POINT('Ctrl Pts',(7.54540514539138,-20.2841925879918,1.26048896755347));
#5349=CARTESIAN_POINT('Ctrl Pts',(7.55524713666923,-20.2853649424747,1.25172099073438));
#5350=CARTESIAN_POINT('Ctrl Pts',(7.5650019652858,-20.2865674429003,1.2428865800128));
#5351=CARTESIAN_POINT('Ctrl Pts',(7.57466753434566,-20.2877995817719,1.2339885196899));
#5352=CARTESIAN_POINT('Ctrl Pts',(7.61835151381923,-20.2933682895055,1.19377333090042));
#5353=CARTESIAN_POINT('Ctrl Pts',(7.66088951452129,-20.3000469589609,1.15186853252888));
#5354=CARTESIAN_POINT('Ctrl Pts',(7.70201667224603,-20.3078244592172,1.1084685010314));
#5355=CARTESIAN_POINT('Ctrl Pts',(7.74315819270392,-20.3156046755901,1.06505331305083));
#5356=CARTESIAN_POINT('Ctrl Pts',(7.78288720787508,-20.3244844830689,1.02014229787602));
#5357=CARTESIAN_POINT('Ctrl Pts',(7.8209637992374,-20.334427858936,0.97396820682318));
#5358=CARTESIAN_POINT('Ctrl Pts',(7.85907418536895,-20.3443800600178,0.92775313408853));
#5359=CARTESIAN_POINT('Ctrl Pts',(7.89552862651523,-20.3553976202851,0.880273333152214));
#5360=CARTESIAN_POINT('Ctrl Pts',(7.93012136692561,-20.3674202884528,0.83179256319971));
#5361=CARTESIAN_POINT('Ctrl Pts',(7.96468775867802,-20.379433799174,0.783348720163393));
#5362=CARTESIAN_POINT('Ctrl Pts',(7.99739485206479,-20.3924506968192,0.733906126191045));
#5363=CARTESIAN_POINT('Ctrl Pts',(8.0280797616722,-20.4063889661352,0.68374857230742));
#5364=CARTESIAN_POINT('Ctrl Pts',(8.05874719517115,-20.4203192971289,0.633619584871035));
#5365=CARTESIAN_POINT('Ctrl Pts',(8.0873944899417,-20.4351696910629,0.582777184219427));
#5366=CARTESIAN_POINT('Ctrl Pts',(8.11390660288973,-20.4508397777779,0.531514551846599));
#5367=CARTESIAN_POINT('Ctrl Pts',(8.11977326376511,-20.4543072903381,0.520171039532054));
#5368=CARTESIAN_POINT('Ctrl Pts',(8.1255355657252,-20.4578148771029,0.508806964005077));
#5369=CARTESIAN_POINT('Ctrl Pts',(8.13119259206894,-20.46136134919,0.49742551165457));
#5370=CARTESIAN_POINT('Ctrl Pts',(8.15675978021637,-20.4773897912725,0.445986519513652));
#5371=CARTESIAN_POINT('Ctrl Pts',(8.18067882422748,-20.4948181203855,0.393696645408831));
#5372=CARTESIAN_POINT('Ctrl Pts',(8.20277709273188,-20.5135819549554,0.340828125587841));
#5373=CARTESIAN_POINT('Ctrl Pts',(8.22488307855853,-20.5323523423717,0.287941142627803));
#5374=CARTESIAN_POINT('Ctrl Pts',(8.24516655941384,-20.5524590343221,0.234475768276538));
#5375=CARTESIAN_POINT('Ctrl Pts',(8.26349134892837,-20.5738061183028,0.180724039814232));
#5376=CARTESIAN_POINT('Ctrl Pts',(8.28183240255724,-20.5951721488266,0.126924604159598));
#5377=CARTESIAN_POINT('Ctrl Pts',(8.2982109611232,-20.6177805253058,0.0728390372979704));
#5378=CARTESIAN_POINT('Ctrl Pts',(8.31253307602321,-20.6415064445685,0.0187692206340316));
#5379=CARTESIAN_POINT('Ctrl Pts',(8.32684428203008,-20.6652142922321,-0.0352594120388522));
#5380=CARTESIAN_POINT('Ctrl Pts',(8.339102027964,-20.6900376261338,-0.0892715721457783));
#5381=CARTESIAN_POINT('Ctrl Pts',(8.34925864520913,-20.7158279105711,-0.142968160449627));
#5382=CARTESIAN_POINT('Ctrl Pts',(8.35940947791238,-20.7416035065568,-0.196634166704727));
#5383=CARTESIAN_POINT('Ctrl Pts',(8.36746160014214,-20.7683445289011,-0.249984259986978));
#5384=CARTESIAN_POINT('Ctrl Pts',(8.37341437361217,-20.7958845557979,-0.302732839445703));
#5385=CARTESIAN_POINT('Ctrl Pts',(8.37473161691483,-20.801978675819,-0.314405165524747));
#5386=CARTESIAN_POINT('Ctrl Pts',(8.37594624412355,-20.8081118638264,-0.326048111329758));
#5387=CARTESIAN_POINT('Ctrl Pts',(8.37705855294184,-20.8142822298008,-0.337658719487504));
#5388=CARTESIAN_POINT('Ctrl Pts',(8.38208568329347,-20.842169479781,-0.390133391728609));
#5389=CARTESIAN_POINT('Ctrl Pts',(8.38532738969146,-20.871535875331,-0.442451690707123));
#5390=CARTESIAN_POINT('Ctrl Pts',(8.38672339583334,-20.9022521666488,-0.494317440111339));
#5391=CARTESIAN_POINT('Ctrl Pts',(8.3881198894989,-20.9329791849392,-0.54620130245975));
#5392=CARTESIAN_POINT('Ctrl Pts',(8.3876692117264,-20.9650567489548,-0.597631562887862));
#5393=CARTESIAN_POINT('Ctrl Pts',(8.38535091254483,-20.9983221257512,-0.648314739716445));
#5394=CARTESIAN_POINT('Ctrl Pts',(8.38303055576349,-21.0316170271372,-0.69904290025303));
#5395=CARTESIAN_POINT('Ctrl Pts',(8.37883922391101,-21.0661014353867,-0.749021923207224));
#5396=CARTESIAN_POINT('Ctrl Pts',(8.37279802773292,-21.101584117782,-0.797971596269669));
#5397=CARTESIAN_POINT('Ctrl Pts',(8.36676143302354,-21.1370397736666,-0.846883985260829));
#5398=CARTESIAN_POINT('Ctrl Pts',(8.35887791922486,-21.1734916692967,-0.894767940777761));
#5399=CARTESIAN_POINT('Ctrl Pts',(8.34920937659625,-21.2107280151238,-0.941368295643095));
#5400=CARTESIAN_POINT('Ctrl Pts',(8.33954634053429,-21.2479431535748,-0.987942110007974));
#5401=CARTESIAN_POINT('Ctrl Pts',(8.3281005770854,-21.2859412854642,-1.03323325565063));
#5402=CARTESIAN_POINT('Ctrl Pts',(8.31497167467398,-21.3244981230677,-1.07702027911484));
#5403=CARTESIAN_POINT('Ctrl Pts',(8.31206648117728,-21.3330300681115,-1.08670957162552));
#5404=CARTESIAN_POINT('Ctrl Pts',(8.30907900829624,-21.3415893397368,-1.09632535949929));
#5405=CARTESIAN_POINT('Ctrl Pts',(8.30601056182147,-21.350173465905,-1.10586550012264));
#5406=CARTESIAN_POINT('Ctrl Pts',(8.2921425782613,-21.3889698149884,-1.14898260006691));
#5407=CARTESIAN_POINT('Ctrl Pts',(8.27674396642908,-21.4290982032865,-1.19096704316453));
#5408=CARTESIAN_POINT('Ctrl Pts',(8.25986467402369,-21.47036574314,-1.23155737439074));
#5409=CARTESIAN_POINT('Ctrl Pts',(8.24297948690575,-21.511647694752,-1.27216188087552));
#5410=CARTESIAN_POINT('Ctrl Pts',(8.22461268059718,-21.5540691404009,-1.31137063355186));
#5411=CARTESIAN_POINT('Ctrl Pts',(8.20484862275808,-21.5974068306545,-1.34894683398735));
#5412=CARTESIAN_POINT('Ctrl Pts',(8.18506702338624,-21.6407829851505,-1.38655638507153));
#5413=CARTESIAN_POINT('Ctrl Pts',(8.16388591234771,-21.6850764469865,-1.42252990566971));
#5414=CARTESIAN_POINT('Ctrl Pts',(8.1414219230224,-21.7300408334262,-1.45666435205228));
#5415=CARTESIAN_POINT('Ctrl Pts',(8.11897504410718,-21.7749709713145,-1.49077279885092));
#5416=CARTESIAN_POINT('Ctrl Pts',(8.09524758180244,-21.8205703748796,-1.52304454512955));
#5417=CARTESIAN_POINT('Ctrl Pts',(8.07038362784117,-21.8665797955301,-1.55331889475944));
#5418=CARTESIAN_POINT('Ctrl Pts',(8.04553383475438,-21.9125630122376,-1.58357600210897));
#5419=CARTESIAN_POINT('Ctrl Pts',(8.01954926787334,-21.9589551262024,-1.61183773325823));
#5420=CARTESIAN_POINT('Ctrl Pts',(7.99259571310654,-22.0054936305649,-1.63799064371839));
#5421=CARTESIAN_POINT('Ctrl Pts',(7.98663136897745,-22.0157917770496,-1.64377781944758));
#5422=CARTESIAN_POINT('Ctrl Pts',(7.98061964812713,-22.0260970990538,-1.64946192467182));
#5423=CARTESIAN_POINT('Ctrl Pts',(7.97456245845175,-22.0364067769132,-1.65504205590818));
#5424=CARTESIAN_POINT('Ctrl Pts',(7.94718671390738,-22.0830018354371,-1.68026171311512));
#5425=CARTESIAN_POINT('Ctrl Pts',(7.91887674686191,-22.1305845981431,-1.70359676647099));
#5426=CARTESIAN_POINT('Ctrl Pts',(7.88976876673361,-22.1789123741453,-1.72487226661212));
#5427=CARTESIAN_POINT('Ctrl Pts',(7.86065062129931,-22.227257027534,-1.74615519674214));
#5428=CARTESIAN_POINT('Ctrl Pts',(7.83073422553015,-22.2763466317668,-1.76537666733516));
#5429=CARTESIAN_POINT('Ctrl Pts',(7.80017708553268,-22.3259157109097,-1.78240346403927));
#5430=CARTESIAN_POINT('Ctrl Pts',(7.76959282463327,-22.3755287849466,-1.79944537282796));
#5431=CARTESIAN_POINT('Ctrl Pts',(7.7383670797749,-22.4256215188224,-1.81428839412937));
#5432=CARTESIAN_POINT('Ctrl Pts',(7.70667355082844,-22.4759145824468,-1.82684686809449));
#5433=CARTESIAN_POINT('Ctrl Pts',(7.67500416226361,-22.526169338764,-1.83939577649957));
#5434=CARTESIAN_POINT('Ctrl Pts',(7.64286815099418,-22.5766234203374,-1.84966349840248));
#5435=CARTESIAN_POINT('Ctrl Pts',(7.61044817181519,-22.6269953141814,-1.85761563656225));
#5436=CARTESIAN_POINT('Ctrl Pts',(7.57804665692642,-22.677338519504,-1.86556324570655));
#5437=CARTESIAN_POINT('Ctrl Pts',(7.54536195718654,-22.7275989569782,-1.87119797990071));
#5438=CARTESIAN_POINT('Ctrl Pts',(7.51257891553807,-22.7775031171609,-1.87453687269564));
#5439=CARTESIAN_POINT('Ctrl Pts',(7.50532460924368,-22.7885460236493,-1.87527571051545));
#5440=CARTESIAN_POINT('Ctrl Pts',(7.49806548194417,-22.7995715361032,-1.87590232633983));
#5441=CARTESIAN_POINT('Ctrl Pts',(7.49080351840538,-22.8105767904773,-1.87641723476232));
#5442=CARTESIAN_POINT('Ctrl Pts',(7.45798274352922,-22.8603155387289,-1.87874438682333));
#5443=CARTESIAN_POINT('Ctrl Pts',(7.42504763653484,-22.9105686272294,-1.87880825693467));
#5444=CARTESIAN_POINT('Ctrl Pts',(7.3921796210866,-22.9610672606356,-1.8765550522609));
#5445=CARTESIAN_POINT('Ctrl Pts',(7.35930012722452,-23.0115835295518,-1.87430106070616));
#5446=CARTESIAN_POINT('Ctrl Pts',(7.32648821890885,-23.0623448587329,-1.86972820122924));
#5447=CARTESIAN_POINT('Ctrl Pts',(7.29392837554156,-23.1130701992057,-1.86283322829495));
#5448=CARTESIAN_POINT('Ctrl Pts',(7.26133963377882,-23.1638405608087,-1.85593213574724));
#5449=CARTESIAN_POINT('Ctrl Pts',(7.22900386338403,-23.2145741682268,-1.8467048153454));
#5450=CARTESIAN_POINT('Ctrl Pts',(7.19710207185721,-23.264987472308,-1.83519995710469));
#5451=CARTESIAN_POINT('Ctrl Pts',(7.16522457934186,-23.3153623774971,-1.82370386190419));
#5452=CARTESIAN_POINT('Ctrl Pts',(7.13378083489573,-23.3654167786337,-1.80993391118305));
#5453=CARTESIAN_POINT('Ctrl Pts',(7.10294078007701,-23.414876502723,-1.79398881938346));
#5454=CARTESIAN_POINT('Ctrl Pts',(7.07211828972738,-23.4643080578029,-1.77805280886061));
#5455=CARTESIAN_POINT('Ctrl Pts',(7.041899171186,-23.5131449913085,-1.75994451788714));
#5456=CARTESIAN_POINT('Ctrl Pts',(7.01243640949997,-23.5611321869611,-1.73980808435003));
#5457=CARTESIAN_POINT('Ctrl Pts',(7.00591682233549,-23.5717509031619,-1.73535224836881));
#5458=CARTESIAN_POINT('Ctrl Pts',(6.99943419425352,-23.5823281035833,-1.73079726584419));
#5459=CARTESIAN_POINT('Ctrl Pts',(6.99299004642871,-23.5928611918346,-1.72614496752462));
#5460=CARTESIAN_POINT('Ctrl Pts',(6.96386542690896,-23.6404659637964,-1.70511869343326));
#5461=CARTESIAN_POINT('Ctrl Pts',(6.93550746092023,-23.6880764387054,-1.68189873004107));
#5462=CARTESIAN_POINT('Ctrl Pts',(6.90809278366361,-23.735426585839,-1.6565630953716));
#5463=CARTESIAN_POINT('Ctrl Pts',(6.88066853244884,-23.7827932689443,-1.63121861280275));
#5464=CARTESIAN_POINT('Ctrl Pts',(6.85418868027218,-23.829898783809,-1.60375713415761));
#5465=CARTESIAN_POINT('Ctrl Pts',(6.82881317228806,-23.8764762463144,-1.57430602553571));
#5466=CARTESIAN_POINT('Ctrl Pts',(6.80341514234476,-23.9230950485127,-1.54482877766699));
#5467=CARTESIAN_POINT('Ctrl Pts',(6.77912380886821,-23.9691841981106,-1.51335869953315));
#5468=CARTESIAN_POINT('Ctrl Pts',(6.7560762807602,-24.0144854908235,-1.48006918735899));
#5469=CARTESIAN_POINT('Ctrl Pts',(6.73304630753319,-24.0597522783696,-1.44680503119794));
#5470=CARTESIAN_POINT('Ctrl Pts',(6.71125853376405,-24.1042318022364,-1.41172471547066));
#5471=CARTESIAN_POINT('Ctrl Pts',(6.69082142948761,-24.1476853800295,-1.3750405146966));
#5472=CARTESIAN_POINT('Ctrl Pts',(6.67039596484308,-24.1911142095195,-1.33837720683323));
#5473=CARTESIAN_POINT('Ctrl Pts',(6.65131980296306,-24.233517753997,-1.30011245980331));
#5474=CARTESIAN_POINT('Ctrl Pts',(6.63366946591674,-24.2746850431039,-1.26048896755363));
#5475=CARTESIAN_POINT('Ctrl Pts',(6.62976375904222,-24.2837946348158,-1.25172099073449));
#5476=CARTESIAN_POINT('Ctrl Pts',(6.6259277406506,-24.2928438144202,-1.24288658001286));
#5477=CARTESIAN_POINT('Ctrl Pts',(6.62216201968439,-24.3018305122039,-1.2339885196899));
#5478=CARTESIAN_POINT('Ctrl Pts',(6.60514267231111,-24.3424463020333,-1.19377333090037));
#5479=CARTESIAN_POINT('Ctrl Pts',(6.58965756937198,-24.3826246259952,-1.15186853252877));
#5480=CARTESIAN_POINT('Ctrl Pts',(6.57582950330943,-24.4221305394985,-1.10846850103124));
#5481=CARTESIAN_POINT('Ctrl Pts',(6.56199660810645,-24.4616502495516,-1.06505331305081));
#5482=CARTESIAN_POINT('Ctrl Pts',(6.54982223937827,-24.5004964896965,-1.02014229787617));
#5483=CARTESIAN_POINT('Ctrl Pts',(6.53939515979743,-24.5384434730392,-0.973968206823508));
#5484=CARTESIAN_POINT('Ctrl Pts',(6.52895882569208,-24.5764241361179,-0.927753134089022));
#5485=CARTESIAN_POINT('Ctrl Pts',(6.52027309219813,-24.6135033883649,-0.880273333152876));
#5486=CARTESIAN_POINT('Ctrl Pts',(6.51338865804746,-24.6494729144305,-0.831792563200549));
#5487=CARTESIAN_POINT('Ctrl Pts',(6.50650946764445,-24.6854150431657,-0.783348720164519));
#5488=CARTESIAN_POINT('Ctrl Pts',(6.50142888499027,-24.720248665745,-0.733906126192465));
#5489=CARTESIAN_POINT('Ctrl Pts',(6.49815732549905,-24.7537917116357,-0.683748572309139));
#5490=CARTESIAN_POINT('Ctrl Pts',(6.49488762927314,-24.7873156536116,-0.633619584872594));
#5491=CARTESIAN_POINT('Ctrl Pts',(6.49342480029085,-24.8195501355998,-0.582777184220826));
#5492=CARTESIAN_POINT('Ctrl Pts',(6.4937394369915,-24.8503453422784,-0.531514551847826));
#5493=CARTESIAN_POINT('Ctrl Pts',(6.49380906051888,-24.8571597759122,-0.520171039532874));
#5494=CARTESIAN_POINT('Ctrl Pts',(6.49396556878318,-24.8639038691766,-0.508806964005485));
#5495=CARTESIAN_POINT('Ctrl Pts',(6.49420839053254,-24.8705762337439,-0.497425511654569));
#5496=CARTESIAN_POINT('Ctrl Pts',(6.49530583448538,-24.9007322892242,-0.445986519513661));
#5497=CARTESIAN_POINT('Ctrl Pts',(6.49843968823718,-24.9301609535285,-0.393696645408851));
#5498=CARTESIAN_POINT('Ctrl Pts',(6.50364051139493,-24.9586805327179,-0.34082812558787));
#5499=CARTESIAN_POINT('Ctrl Pts',(6.508843150823,-24.9872100717278,-0.287941142627552));
#5500=CARTESIAN_POINT('Ctrl Pts',(6.51611431641051,-25.014829427401,-0.234475768275999));
#5501=CARTESIAN_POINT('Ctrl Pts',(6.52543903867732,-25.0413727026301,-0.180724039813404));
#5502=CARTESIAN_POINT('Ctrl Pts',(6.5347720370746,-25.0679395362668,-0.126924604158596));
#5503=CARTESIAN_POINT('Ctrl Pts',(6.54616218616096,-25.093427972302,-0.0728390372967965));
#5504=CARTESIAN_POINT('Ctrl Pts',(6.55954837752067,-25.1176942472727,-0.0187692206326862));
#5505=CARTESIAN_POINT('Ctrl Pts',(6.57292437286312,-25.1419420390654,0.0352594120404618));
#5506=CARTESIAN_POINT('Ctrl Pts',(6.58829313766177,-25.1649692253883,0.0892715721476517));
#5507=CARTESIAN_POINT('Ctrl Pts',(6.60554987053284,-25.1866602561578,0.142968160451755));
#5508=CARTESIAN_POINT('Ctrl Pts',(6.62279677510259,-25.2083389331412,0.196634166706848));
#5509=CARTESIAN_POINT('Ctrl Pts',(6.64192911866103,-25.2286827867186,0.249984259989086));
#5510=CARTESIAN_POINT('Ctrl Pts',(6.66280309483961,-25.247608053215,0.302732839447797));
#5511=CARTESIAN_POINT('Ctrl Pts',(6.66742213594002,-25.2517958793884,0.314405165526138));
#5512=CARTESIAN_POINT('Ctrl Pts',(6.67212631895598,-25.2559143714107,0.326048111330451));
#5513=CARTESIAN_POINT('Ctrl Pts',(6.67691385823105,-25.2599628420912,0.337658719487501));
#5514=CARTESIAN_POINT('Ctrl Pts',(6.69855135997981,-25.2782600896739,0.39013339172883));
#5515=CARTESIAN_POINT('Ctrl Pts',(6.72236255134487,-25.2957506875413,0.442451690707569));
#5516=CARTESIAN_POINT('Ctrl Pts',(6.7482656368653,-25.312317809983,0.494317440112001));
#5517=CARTESIAN_POINT('Ctrl Pts',(6.77417776845468,-25.3288907181188,0.546201302460738));
#5518=CARTESIAN_POINT('Ctrl Pts',(6.80218309267025,-25.3445392017269,0.59763156288917));
#5519=CARTESIAN_POINT('Ctrl Pts',(6.8321509036334,-25.3591641841403,0.648314739718059));
#5520=CARTESIAN_POINT('Ctrl Pts',(6.86214531244092,-25.3738021469148,0.699042900254681));
#5521=CARTESIAN_POINT('Ctrl Pts',(6.89410535194574,-25.3874145511796,0.749021923208903));
#5522=CARTESIAN_POINT('Ctrl Pts',(6.92785485438357,-25.3999240630178,0.797971596271375));
#5523=CARTESIAN_POINT('Ctrl Pts',(6.96157865044198,-25.4124240465893,0.84688398526218));
#5524=CARTESIAN_POINT('Ctrl Pts',(6.9970886749729,-25.4238226711835,0.894767940778771));
#5525=CARTESIAN_POINT('Ctrl Pts',(7.03417056771735,-25.434067640563,0.941368295643777));
#5526=CARTESIAN_POINT('Ctrl Pts',(7.07123134105188,-25.4443067750811,0.987942110008198));
#5527=CARTESIAN_POINT('Ctrl Pts',(7.10986157028853,-25.4533935191132,1.03323325565042));
#5528=CARTESIAN_POINT('Ctrl Pts',(7.14981722234809,-25.4613019749028,1.07702027911423));
#5529=CARTESIAN_POINT('Ctrl Pts',(7.15865870024823,-25.4630519760537,1.08670957162511));
#5530=CARTESIAN_POINT('Ctrl Pts',(7.16756498335432,-25.4647443844583,1.09632535949909));
#5531=CARTESIAN_POINT('Ctrl Pts',(7.17653327792285,-25.4663790949451,1.10586550012264));
#5532=CARTESIAN_POINT('Ctrl Pts',(7.21706589358342,-25.4737672434245,1.14898260006703));
#5533=CARTESIAN_POINT('Ctrl Pts',(7.2595174031787,-25.4804958485438,1.19096704316477));
#5534=CARTESIAN_POINT('Ctrl Pts',(7.30369578724639,-25.4865117224496,1.23155737439109));
#5535=CARTESIAN_POINT('Ctrl Pts',(7.34788959961906,-25.4925296972638,1.2721618808758));
#5536=CARTESIAN_POINT('Ctrl Pts',(7.39381105237047,-25.4978342992387,1.31137063355205));
#5537=CARTESIAN_POINT('Ctrl Pts',(7.4412246219909,-25.5023869681949,1.34894683398747));
#5538=CARTESIAN_POINT('Ctrl Pts',(7.48868027338876,-25.5069436778594,1.38655638507158));
#5539=CARTESIAN_POINT('Ctrl Pts',(7.53763009207947,-25.5107470285377,1.42252990566968));
#5540=CARTESIAN_POINT('Ctrl Pts',(7.58780238766435,-25.5137748363314,1.45666435205219));
#5541=CARTESIAN_POINT('Ctrl Pts',(7.63793646792892,-25.5168003378994,1.49077279885092));
#5542=CARTESIAN_POINT('Ctrl Pts',(7.68929044096624,-25.5190514545587,1.52304454512963));
#5543=CARTESIAN_POINT('Ctrl Pts',(7.74156774504371,-25.5205233491149,1.5533188947596));
#5544=CARTESIAN_POINT('Ctrl Pts',(7.7938152754032,-25.5219944053767,1.58357600210892));
#5545=CARTESIAN_POINT('Ctrl Pts',(7.84698430807213,-25.5226871673338,1.61183773325798));
#5546=CARTESIAN_POINT('Ctrl Pts',(7.90076461248722,-25.5226139563647,1.63799064371799));
#5547=CARTESIAN_POINT('Ctrl Pts',(7.91266524101966,-25.5225977560744,1.64377781944732));
#5548=CARTESIAN_POINT('Ctrl Pts',(7.92459577209495,-25.5225441140996,1.64946192467169));
#5549=CARTESIAN_POINT('Ctrl Pts',(7.936552809864,-25.5224532728949,1.65504205590817));
#5550=CARTESIAN_POINT('Ctrl Pts',(7.99059318650879,-25.5220427119339,1.6802617131152));
#5551=CARTESIAN_POINT('Ctrl Pts',(8.04595605131735,-25.5213169426452,1.70359676647112));
#5552=CARTESIAN_POINT('Ctrl Pts',(8.10236312310797,-25.5202725804024,1.7248722666123));
#5553=CARTESIAN_POINT('Ctrl Pts',(8.15878989379704,-25.5192278534395,1.74615519674236));
#5554=CARTESIAN_POINT('Ctrl Pts',(8.21626093600908,-25.5178642968302,1.7653766673354));
#5555=CARTESIAN_POINT('Ctrl Pts',(8.27446758778794,-25.5161855768968,1.78240346403954));
#5556=CARTESIAN_POINT('Ctrl Pts',(8.33272590071357,-25.5145053670204,1.79944537282824));
#5557=CARTESIAN_POINT('Ctrl Pts',(8.39172035322431,-25.5125094456588,1.81428839412965));
#5558=CARTESIAN_POINT('Ctrl Pts',(8.45112218843054,-25.5102085762678,1.82684686809477));
#5559=CARTESIAN_POINT('Ctrl Pts',(8.51047877834426,-25.5079094594069,1.83939577649973));
#5560=CARTESIAN_POINT('Ctrl Pts',(8.57024130034582,-25.5053058980581,1.84966349840256));
#5561=CARTESIAN_POINT('Ctrl Pts',(8.63007462964054,-25.5024153194209,1.85761563656227));
#5562=CARTESIAN_POINT('Ctrl Pts',(8.68987388180219,-25.4995263870674,1.86556324570657));
#5563=CARTESIAN_POINT('Ctrl Pts',(8.74974304733016,-25.4963508255147,1.87119797990072));
#5564=CARTESIAN_POINT('Ctrl Pts',(8.80935283862714,-25.4929119587252,1.87453687269564));
#5565=CARTESIAN_POINT('Ctrl Pts',(8.82254342932487,-25.4921509984316,1.87527571051545));
#5566=CARTESIAN_POINT('Ctrl Pts',(8.83572136684934,-25.4913771660079,1.87590232633983));
#5567=CARTESIAN_POINT('Ctrl Pts',(8.84888317848179,-25.490590748289,1.87641723476232));
#5568=CARTESIAN_POINT('Ctrl Pts',(8.90836858545845,-25.4870364976001,1.87874438682334));
#5569=CARTESIAN_POINT('Ctrl Pts',(8.968356590216,-25.4836404025168,1.87880825693467));
#5570=CARTESIAN_POINT('Ctrl Pts',(9.02852369732664,-25.4804251828698,1.87655505226086));
#5571=CARTESIAN_POINT('Ctrl Pts',(9.08871181644355,-25.4772088403798,1.8743010607061));
#5572=CARTESIAN_POINT('Ctrl Pts',(9.14907837120213,-25.4741735588223,1.86972820122916));
#5573=CARTESIAN_POINT('Ctrl Pts',(9.20928772635084,-25.4713385775594,1.86283322829483));
#5574=CARTESIAN_POINT('Ctrl Pts',(9.26955052013971,-25.468501080117,1.85593213574709));
#5575=CARTESIAN_POINT('Ctrl Pts',(9.32965499818679,-25.4658642852132,1.84670481534523));
#5576=CARTESIAN_POINT('Ctrl Pts',(9.38926509597328,-25.4634431753654,1.83519995710449));
#5577=CARTESIAN_POINT('Ctrl Pts',(9.44882978983824,-25.4610239096326,1.82370386190391));
#5578=CARTESIAN_POINT('Ctrl Pts',(9.5079000450172,-25.4588200287205,1.80993391118265));
#5579=CARTESIAN_POINT('Ctrl Pts',(9.56615344995236,-25.456841619838,1.79398881938292));
#5580=CARTESIAN_POINT('Ctrl Pts',(9.62437367757489,-25.4548643377273,1.77805280886001));
#5581=CARTESIAN_POINT('Ctrl Pts',(9.68177726190438,-25.4531122801433,1.75994451788648));
#5582=CARTESIAN_POINT('Ctrl Pts',(9.73806677323893,-25.4515903778838,1.73980808434933));
#5583=CARTESIAN_POINT('Ctrl Pts',(9.75052264480599,-25.4512536078776,1.73535224836833));
#5584=CARTESIAN_POINT('Ctrl Pts',(9.76292408311216,-25.4509280874861,1.73079726584394));
#5585=CARTESIAN_POINT('Ctrl Pts',(9.77526807902988,-25.4506138358897,1.72614496752462));
#5586=CARTESIAN_POINT('Ctrl Pts',(9.83105733064982,-25.449193561491,1.70511869343333));
#5587=CARTESIAN_POINT('Ctrl Pts',(9.8864681944014,-25.4484400799996,1.68189873004125));
#5588=CARTESIAN_POINT('Ctrl Pts',(9.94118196332011,-25.4483733466256,1.65656309537189));
#5589=CARTESIAN_POINT('Ctrl Pts',(9.99591483978936,-25.4483065899465,1.63121861280321));
#5590=CARTESIAN_POINT('Ctrl Pts',(10.0499493384086,-25.4489271227054,1.60375713415827));
#5591=CARTESIAN_POINT('Ctrl Pts',(10.1029743581738,-25.4502400194099,1.57430602553659));
#5592=CARTESIAN_POINT('Ctrl Pts',(10.1560464401432,-25.451554081372,1.54482877766791));
#5593=CARTESIAN_POINT('Ctrl Pts',(10.2081064812721,-25.4535617442885,1.51335869953411));
#5594=CARTESIAN_POINT('Ctrl Pts',(10.2588623156398,-25.4562526458089,1.48006918735998));
#5595=CARTESIAN_POINT('Ctrl Pts',(10.3095794902161,-25.4589414977189,1.44680503119883));
#5596=CARTESIAN_POINT('Ctrl Pts',(10.3589937747178,-25.4623124940763,1.41172471547144));
#5597=CARTESIAN_POINT('Ctrl Pts',(10.4068442291104,-25.4663402314897,1.37504051469726));
#5598=CARTESIAN_POINT('Ctrl Pts',(10.4546674310282,-25.4703656749685,1.33837720683351));
#5599=CARTESIAN_POINT('Ctrl Pts',(10.5009280586967,-25.4750470064124,1.30011245980319));
#5600=CARTESIAN_POINT('Ctrl Pts',(10.5454051453918,-25.4803450106985,1.26048896755308));
#5601=CARTESIAN_POINT('Ctrl Pts',(10.5552471366695,-25.4815173651814,1.25172099073412));
#5602=CARTESIAN_POINT('Ctrl Pts',(10.5650019652859,-25.482719865607,1.24288658001267));
#5603=CARTESIAN_POINT('Ctrl Pts',(10.5746675343456,-25.4839520044785,1.2339885196899));
#5604=CARTESIAN_POINT('Ctrl Pts',(10.6183515138194,-25.4895207122121,1.19377333090027));
#5605=CARTESIAN_POINT('Ctrl Pts',(10.6608895145216,-25.4961993816676,1.15186853252856));
#5606=CARTESIAN_POINT('Ctrl Pts',(10.7020166722465,-25.5039768819239,1.10846850103091));
#5607=CARTESIAN_POINT('Ctrl Pts',(10.7431581927042,-25.5117570982968,1.06505331305044));
#5608=CARTESIAN_POINT('Ctrl Pts',(10.7828872078753,-25.5206369057756,1.02014229787575));
#5609=CARTESIAN_POINT('Ctrl Pts',(10.8209637992375,-25.5305802816427,0.973968206823044));
#5610=CARTESIAN_POINT('Ctrl Pts',(10.859074185369,-25.5405324827245,0.927753134088394));
#5611=CARTESIAN_POINT('Ctrl Pts',(10.8955286265153,-25.5515500429918,0.880273333152076));
#5612=CARTESIAN_POINT('Ctrl Pts',(10.9301213669257,-25.5635727111595,0.831792563199574));
#5613=CARTESIAN_POINT('Ctrl Pts',(10.9646877586782,-25.5755862218807,0.783348720163117));
#5614=CARTESIAN_POINT('Ctrl Pts',(10.997394852065,-25.5886031195259,0.733906126190626));
#5615=CARTESIAN_POINT('Ctrl Pts',(11.0280797616725,-25.6025413888421,0.683748572306851));
#5616=CARTESIAN_POINT('Ctrl Pts',(11.0587471951712,-25.6164717198356,0.633619584870804));
#5617=CARTESIAN_POINT('Ctrl Pts',(11.0873944899416,-25.6313221137695,0.582777184219545));
#5618=CARTESIAN_POINT('Ctrl Pts',(11.1139066028895,-25.6469922004844,0.531514551847072));
#5619=CARTESIAN_POINT('Ctrl Pts',(11.1197732637649,-25.6504597130446,0.520171039532368));
#5620=CARTESIAN_POINT('Ctrl Pts',(11.1255355657251,-25.6539672998095,0.508806964005237));
#5621=CARTESIAN_POINT('Ctrl Pts',(11.1311925920689,-25.6575137718966,0.497425511654571));
#5622=CARTESIAN_POINT('Ctrl Pts',(11.1567597802163,-25.6735422139791,0.445986519513735));
#5623=CARTESIAN_POINT('Ctrl Pts',(11.1806788242274,-25.6909705430921,0.393696645409006));
#5624=CARTESIAN_POINT('Ctrl Pts',(11.2027770927317,-25.709734377662,0.340828125588102));
#5625=CARTESIAN_POINT('Ctrl Pts',(11.2248830785586,-25.7285047650784,0.287941142627488));
#5626=CARTESIAN_POINT('Ctrl Pts',(11.2451665594142,-25.7486114570291,0.234475768275634));
#5627=CARTESIAN_POINT('Ctrl Pts',(11.2634913489288,-25.76995854101,0.180724039812736));
#5628=CARTESIAN_POINT('Ctrl Pts',(11.2818324025577,-25.7913245715339,0.126924604158014));
#5629=CARTESIAN_POINT('Ctrl Pts',(11.2982109611237,-25.8139329480131,0.0728390372962978));
#5630=CARTESIAN_POINT('Ctrl Pts',(11.3125330760236,-25.8376588672759,0.0187692206322746));
#5631=CARTESIAN_POINT('Ctrl Pts',(11.3268442820305,-25.8613667149396,-0.0352594120405529));
#5632=CARTESIAN_POINT('Ctrl Pts',(11.3391020279643,-25.8861900488413,-0.0892715721474228));
#5633=CARTESIAN_POINT('Ctrl Pts',(11.3492586452094,-25.9119803332785,-0.142968160451209));
#5634=CARTESIAN_POINT('Ctrl Pts',(11.3594094779127,-25.9377559292644,-0.196634166706611));
#5635=CARTESIAN_POINT('Ctrl Pts',(11.3674616001424,-25.9644969516088,-0.249984259989154));
#5636=CARTESIAN_POINT('Ctrl Pts',(11.3734143736124,-25.9920369785058,-0.302732839448165));
#5637=CARTESIAN_POINT('Ctrl Pts',(11.374731616915,-25.9981310985265,-0.314405165526383));
#5638=CARTESIAN_POINT('Ctrl Pts',(11.3759462441236,-26.0042642865335,-0.326048111330576));
#5639=CARTESIAN_POINT('Ctrl Pts',(11.3770585529418,-26.0104346525075,-0.337658719487504));
#5640=CARTESIAN_POINT('Ctrl Pts',(11.3820856832934,-26.0383219024876,-0.390133391728687));
#5641=CARTESIAN_POINT('Ctrl Pts',(11.3853273896914,-26.0676882980378,-0.442451690707274));
#5642=CARTESIAN_POINT('Ctrl Pts',(11.3867233958333,-26.0984045893556,-0.494317440111565));
#5643=CARTESIAN_POINT('Ctrl Pts',(11.3881198894989,-26.1291316076458,-0.54620130245979));
#5644=CARTESIAN_POINT('Ctrl Pts',(11.3876692117264,-26.1612091716614,-0.597631562887722));
#5645=CARTESIAN_POINT('Ctrl Pts',(11.3853509125448,-26.1944745484577,-0.648314739716127));
#5646=CARTESIAN_POINT('Ctrl Pts',(11.3830305557635,-26.2277694498437,-0.699042900252813));
#5647=CARTESIAN_POINT('Ctrl Pts',(11.378839223911,-26.2622538580933,-0.749021923207109));
#5648=CARTESIAN_POINT('Ctrl Pts',(11.3727980277329,-26.2977365404886,-0.797971596269648));
#5649=CARTESIAN_POINT('Ctrl Pts',(11.3667614330235,-26.3331921963733,-0.846883985261025));
#5650=CARTESIAN_POINT('Ctrl Pts',(11.3588779192248,-26.3696440920036,-0.894767940778162));
#5651=CARTESIAN_POINT('Ctrl Pts',(11.3492093765961,-26.4068804378309,-0.941368295643691));
#5652=CARTESIAN_POINT('Ctrl Pts',(11.3395463405341,-26.4440955762819,-0.987942110008597));
#5653=CARTESIAN_POINT('Ctrl Pts',(11.3281005770852,-26.4820937081714,-1.03323325565127));
#5654=CARTESIAN_POINT('Ctrl Pts',(11.3149716746738,-26.5206505457749,-1.07702027911551));
#5655=CARTESIAN_POINT('Ctrl Pts',(11.3120664811771,-26.5291824908185,-1.08670957162596));
#5656=CARTESIAN_POINT('Ctrl Pts',(11.3090790082961,-26.5377417624436,-1.09632535949951));
#5657=CARTESIAN_POINT('Ctrl Pts',(11.3060105618214,-26.5463258886116,-1.10586550012264));
#5658=CARTESIAN_POINT('Ctrl Pts',(11.2921425782613,-26.5851222376949,-1.14898260006675));
#5659=CARTESIAN_POINT('Ctrl Pts',(11.2767439664292,-26.6252506259928,-1.19096704316423));
#5660=CARTESIAN_POINT('Ctrl Pts',(11.2598646740238,-26.6665181658462,-1.2315573743903));
#5661=CARTESIAN_POINT('Ctrl Pts',(11.2429794869062,-26.7078001174575,-1.27216188087439));
#5662=CARTESIAN_POINT('Ctrl Pts',(11.224612680598,-26.7502215631056,-1.31137063355007));
#5663=CARTESIAN_POINT('Ctrl Pts',(11.2048486227593,-26.7935592533584,-1.34894683398498));
#5664=CARTESIAN_POINT('Ctrl Pts',(11.1850670233875,-26.8369354078544,-1.38655638506922));
#5665=CARTESIAN_POINT('Ctrl Pts',(11.1638859123491,-26.8812288696903,-1.42252990566746));
#5666=CARTESIAN_POINT('Ctrl Pts',(11.1414219230238,-26.9261932561299,-1.4566643520501));
#5667=CARTESIAN_POINT('Ctrl Pts',(11.1189750441086,-26.9711233940183,-1.49077279884888));
#5668=CARTESIAN_POINT('Ctrl Pts',(11.0952475818039,-27.0167227975835,-1.52304454512765));
#5669=CARTESIAN_POINT('Ctrl Pts',(11.0703836278426,-27.062732218234,-1.55331889475767));
#5670=CARTESIAN_POINT('Ctrl Pts',(11.0455338347557,-27.1087154349417,-1.5835760021074));
#5671=CARTESIAN_POINT('Ctrl Pts',(11.0195492678746,-27.1551075489067,-1.61183773325684));
#5672=CARTESIAN_POINT('Ctrl Pts',(10.9925957131078,-27.2016460532694,-1.63799064371718));
#5673=CARTESIAN_POINT('Ctrl Pts',(10.9866313689783,-27.2119441997548,-1.64377781944678));
#5674=CARTESIAN_POINT('Ctrl Pts',(10.9806196481275,-27.2222495217598,-1.64946192467143));
#5675=CARTESIAN_POINT('Ctrl Pts',(10.9745624584517,-27.2325591996199,-1.65504205590817));
#5676=CARTESIAN_POINT('Ctrl Pts',(10.9471867139073,-27.2791542581438,-1.68026171311514));
#5677=CARTESIAN_POINT('Ctrl Pts',(10.9188767468618,-27.3267370208498,-1.70359676647102));
#5678=CARTESIAN_POINT('Ctrl Pts',(10.8897687667335,-27.375064796852,-1.72487226661215));
#5679=CARTESIAN_POINT('Ctrl Pts',(10.860650621299,-27.4234094502411,-1.74615519674231));
#5680=CARTESIAN_POINT('Ctrl Pts',(10.8307342255297,-27.4724990544741,-1.76537666733542));
#5681=CARTESIAN_POINT('Ctrl Pts',(10.800177085532,-27.5220681336174,-1.78240346403961));
#5682=CARTESIAN_POINT('Ctrl Pts',(10.7695928246326,-27.5716812076544,-1.7994453728283));
#5683=CARTESIAN_POINT('Ctrl Pts',(10.7383670797741,-27.6217739415302,-1.81428839412971));
#5684=CARTESIAN_POINT('Ctrl Pts',(10.7066735508276,-27.6720670051547,-1.82684686809482));
#5685=CARTESIAN_POINT('Ctrl Pts',(10.6750041622627,-27.722321761472,-1.83939577649987));
#5686=CARTESIAN_POINT('Ctrl Pts',(10.6428681509933,-27.7727758430455,-1.84966349840274));
#5687=CARTESIAN_POINT('Ctrl Pts',(10.6104481718142,-27.8231477368895,-1.85761563656247));
#5688=CARTESIAN_POINT('Ctrl Pts',(10.5780466569254,-27.8734909422121,-1.86556324570674));
#5689=CARTESIAN_POINT('Ctrl Pts',(10.5453619571855,-27.9237513796864,-1.87119797990086));
#5690=CARTESIAN_POINT('Ctrl Pts',(10.512578915537,-27.9736555398692,-1.87453687269574));
#5691=CARTESIAN_POINT('Ctrl Pts',(10.5053246092429,-27.9846984463571,-1.87527571051551));
#5692=CARTESIAN_POINT('Ctrl Pts',(10.4980654819438,-27.9957239588104,-1.87590232633986));
#5693=CARTESIAN_POINT('Ctrl Pts',(10.4908035184054,-28.0067292131839,-1.87641723476232));
#5694=CARTESIAN_POINT('Ctrl Pts',(10.4579827435293,-28.0564679614354,-1.87874438682332));
#5695=CARTESIAN_POINT('Ctrl Pts',(10.4250476365349,-28.1067210499358,-1.87880825693467));
#5696=CARTESIAN_POINT('Ctrl Pts',(10.3921796210867,-28.157219683342,-1.87655505226091));
#5697=CARTESIAN_POINT('Ctrl Pts',(10.359300127225,-28.2077359522577,-1.8743010607062));
#5698=CARTESIAN_POINT('Ctrl Pts',(10.3264882189097,-28.2584972814382,-1.86972820122937));
#5699=CARTESIAN_POINT('Ctrl Pts',(10.2939283755428,-28.3092226219104,-1.86283322829521));
#5700=CARTESIAN_POINT('Ctrl Pts',(10.26133963378,-28.3599929835134,-1.85593213574756));
#5701=CARTESIAN_POINT('Ctrl Pts',(10.2290038633852,-28.4107265909315,-1.84670481534578));
#5702=CARTESIAN_POINT('Ctrl Pts',(10.1971020718584,-28.4611398950128,-1.83519995710512));
#5703=CARTESIAN_POINT('Ctrl Pts',(10.165224579343,-28.5115148002019,-1.82370386190467));
#5704=CARTESIAN_POINT('Ctrl Pts',(10.1337808348968,-28.5615692013386,-1.80993391118357));
#5705=CARTESIAN_POINT('Ctrl Pts',(10.102940780078,-28.611028925428,-1.79398881938401));
#5706=CARTESIAN_POINT('Ctrl Pts',(10.0721182897286,-28.6604604805075,-1.77805280886132));
#5707=CARTESIAN_POINT('Ctrl Pts',(10.0418991711874,-28.7092974140128,-1.75994451788804));
#5708=CARTESIAN_POINT('Ctrl Pts',(10.0124364095016,-28.7572846096651,-1.73980808435114));
#5709=CARTESIAN_POINT('Ctrl Pts',(10.0059168223365,-28.7679033258668,-1.73535224836956));
#5710=CARTESIAN_POINT('Ctrl Pts',(9.99943419425403,-28.7784805262891,-1.73079726584457));
#5711=CARTESIAN_POINT('Ctrl Pts',(9.99299004642868,-28.7890136145413,-1.72614496752462));
#5712=CARTESIAN_POINT('Ctrl Pts',(9.96386542690912,-28.8366183865028,-1.70511869343339));
#5713=CARTESIAN_POINT('Ctrl Pts',(9.93550746092056,-28.8842288614115,-1.68189873004137));
#5714=CARTESIAN_POINT('Ctrl Pts',(9.90809278366411,-28.9315790085447,-1.65656309537209));
#5715=CARTESIAN_POINT('Ctrl Pts',(9.88066853244946,-28.9789456916498,-1.63121861280338));
#5716=CARTESIAN_POINT('Ctrl Pts',(9.85418868027291,-29.0260512065143,-1.60375713415841));
#5717=CARTESIAN_POINT('Ctrl Pts',(9.82881317228889,-29.0726286690195,-1.57430602553671));
#5718=CARTESIAN_POINT('Ctrl Pts',(9.80341514234551,-29.1192474712179,-1.54482877766797));
#5719=CARTESIAN_POINT('Ctrl Pts',(9.77912380886889,-29.1653366208159,-1.5133586995341));
#5720=CARTESIAN_POINT('Ctrl Pts',(9.7560762807608,-29.2106379135289,-1.48006918735989));
#5721=CARTESIAN_POINT('Ctrl Pts',(9.73304630753345,-29.2559047010756,-1.44680503119842));
#5722=CARTESIAN_POINT('Ctrl Pts',(9.711258533764,-29.3003842249431,-1.41172471547066));
#5723=CARTESIAN_POINT('Ctrl Pts',(9.69082142948729,-29.3438378027368,-1.37504051469608));
#5724=CARTESIAN_POINT('Ctrl Pts',(9.67039596484249,-29.3872666322274,-1.33837720683217));
#5725=CARTESIAN_POINT('Ctrl Pts',(9.65131980296222,-29.4296701767054,-1.30011245980167));
#5726=CARTESIAN_POINT('Ctrl Pts',(9.63366946591571,-29.4708374658129,-1.26048896755137));
#5727=CARTESIAN_POINT('Ctrl Pts',(9.62976375904153,-29.479947057524,-1.25172099073297));
#5728=CARTESIAN_POINT('Ctrl Pts',(9.62592774065024,-29.4889962371276,-1.24288658001209));
#5729=CARTESIAN_POINT('Ctrl Pts',(9.62216201968436,-29.4979829349106,-1.2339885196899));
#5730=CARTESIAN_POINT('Ctrl Pts',(9.6051426723111,-29.5385987247399,-1.19377333090041));
#5731=CARTESIAN_POINT('Ctrl Pts',(9.58965756937199,-29.5787770487018,-1.15186853252886));
#5732=CARTESIAN_POINT('Ctrl Pts',(9.57582950330945,-29.618282962205,-1.10846850103139));
#5733=CARTESIAN_POINT('Ctrl Pts',(9.5619966081064,-29.6578026722583,-1.06505331305076));
#5734=CARTESIAN_POINT('Ctrl Pts',(9.54982223937817,-29.6966489124034,-1.0201422978759));
#5735=CARTESIAN_POINT('Ctrl Pts',(9.53939515979729,-29.7345958957462,-0.973968206823007));
#5736=CARTESIAN_POINT('Ctrl Pts',(9.52895882569192,-29.772576558825,-0.927753134088401));
#5737=CARTESIAN_POINT('Ctrl Pts',(9.52027309219798,-29.8096558110721,-0.880273333152132));
#5738=CARTESIAN_POINT('Ctrl Pts',(9.51338865804731,-29.8456253371378,-0.831792563199677));
#5739=CARTESIAN_POINT('Ctrl Pts',(9.50650946764427,-29.8815674658732,-0.783348720163336));
#5740=CARTESIAN_POINT('Ctrl Pts',(9.5014288849901,-29.9164010884527,-0.733906126190959));
#5741=CARTESIAN_POINT('Ctrl Pts',(9.4981573254989,-29.9499441343436,-0.683748572307306));
#5742=CARTESIAN_POINT('Ctrl Pts',(9.49488762927306,-29.9834680763192,-0.633619584871212));
#5743=CARTESIAN_POINT('Ctrl Pts',(9.49342480029081,-30.015702558307,-0.582777184219908));
#5744=CARTESIAN_POINT('Ctrl Pts',(9.49373943699148,-30.0464977649853,-0.531514551847384));
#5745=CARTESIAN_POINT('Ctrl Pts',(9.49380906051886,-30.053312198619,-0.520171039532578));
#5746=CARTESIAN_POINT('Ctrl Pts',(9.49396556878315,-30.0600562918833,-0.508806964005337));
#5747=CARTESIAN_POINT('Ctrl Pts',(9.49420839053251,-30.0667286564506,-0.497425511654568));
#5748=CARTESIAN_POINT('Ctrl Pts',(9.49530583448534,-30.0968847119308,-0.445986519513711));
#5749=CARTESIAN_POINT('Ctrl Pts',(9.49843968823714,-30.1263133762351,-0.393696645408955));
#5750=CARTESIAN_POINT('Ctrl Pts',(9.50364051139489,-30.1548329554245,-0.34082812558803));
#5751=CARTESIAN_POINT('Ctrl Pts',(9.50884315082298,-30.1833624944346,-0.287941142627382));
#5752=CARTESIAN_POINT('Ctrl Pts',(9.51611431641054,-30.2109818501079,-0.234475768275499));
#5753=CARTESIAN_POINT('Ctrl Pts',(9.52543903867744,-30.2375251253372,-0.180724039812564));
#5754=CARTESIAN_POINT('Ctrl Pts',(9.53477203707472,-30.2640919589739,-0.126924604157851));
#5755=CARTESIAN_POINT('Ctrl Pts',(9.54616218616107,-30.2895803950089,-0.0728390372961486));
#5756=CARTESIAN_POINT('Ctrl Pts',(9.55954837752077,-30.3138466699796,-0.0187692206321375));
#5757=CARTESIAN_POINT('Ctrl Pts',(9.57292437286319,-30.3380944617722,0.0352594120408156));
#5758=CARTESIAN_POINT('Ctrl Pts',(9.58829313766179,-30.361121648095,0.0892715721478093));
#5759=CARTESIAN_POINT('Ctrl Pts',(9.6055498705328,-30.3828126788644,0.142968160451718));
#5760=CARTESIAN_POINT('Ctrl Pts',(9.62279677510249,-30.4044913558477,0.196634166706646));
#5761=CARTESIAN_POINT('Ctrl Pts',(9.64192911866087,-30.4248352094251,0.249984259988728));
#5762=CARTESIAN_POINT('Ctrl Pts',(9.66280309483938,-30.4437604759214,0.30273283944728));
#5763=CARTESIAN_POINT('Ctrl Pts',(9.66742213593985,-30.4479483020949,0.314405165525795));
#5764=CARTESIAN_POINT('Ctrl Pts',(9.67212631895587,-30.4520667941173,0.326048111330278));
#5765=CARTESIAN_POINT('Ctrl Pts',(9.67691385823102,-30.4561152647978,0.3376587194875));
#5766=CARTESIAN_POINT('Ctrl Pts',(9.69855135997969,-30.4744125123805,0.390133391728636));
#5767=CARTESIAN_POINT('Ctrl Pts',(9.72236255134466,-30.4919031102478,0.442451690707181));
#5768=CARTESIAN_POINT('Ctrl Pts',(9.74826563686498,-30.5084702326894,0.494317440111426));
#5769=CARTESIAN_POINT('Ctrl Pts',(9.77417776845419,-30.5250431408252,0.546201302459856));
#5770=CARTESIAN_POINT('Ctrl Pts',(9.80218309266957,-30.5406916244332,0.597631562887992));
#5771=CARTESIAN_POINT('Ctrl Pts',(9.8321509036325,-30.5553166068466,0.648314739716593));
#5772=CARTESIAN_POINT('Ctrl Pts',(9.86214531244,-30.5699545696211,0.699042900253254));
#5773=CARTESIAN_POINT('Ctrl Pts',(9.8941053519448,-30.5835669738859,0.749021923207519));
#5774=CARTESIAN_POINT('Ctrl Pts',(9.92785485438261,-30.5960764857241,0.797971596270033));
#5775=CARTESIAN_POINT('Ctrl Pts',(9.96157865044122,-30.6085764692957,0.846883985261196));
#5776=CARTESIAN_POINT('Ctrl Pts',(9.99708867497237,-30.61997509389,0.894767940778138));
#5777=CARTESIAN_POINT('Ctrl Pts',(10.0341705677171,-30.6302200632696,0.941368295643474));
#5778=CARTESIAN_POINT('Ctrl Pts',(10.071231341052,-30.6404591977878,0.987942110008423));
#5779=CARTESIAN_POINT('Ctrl Pts',(10.1098615702891,-30.64954594182,1.03323325565114));
#5780=CARTESIAN_POINT('Ctrl Pts',(10.1498172223491,-30.6574543976097,1.07702027911541));
#5781=CARTESIAN_POINT('Ctrl Pts',(10.1586587002489,-30.6592043987605,1.0867095716259));
#5782=CARTESIAN_POINT('Ctrl Pts',(10.1675649833546,-30.660896807165,1.09632535949948));
#5783=CARTESIAN_POINT('Ctrl Pts',(10.1765332779228,-30.6625315176518,1.10586550012264));
#5784=CARTESIAN_POINT('Ctrl Pts',(10.2170658935834,-30.6699196661312,1.14898260006707));
#5785=CARTESIAN_POINT('Ctrl Pts',(10.2595174031787,-30.6766482712505,1.19096704316485));
#5786=CARTESIAN_POINT('Ctrl Pts',(10.3036957872465,-30.6826641451563,1.2315573743912));
#5787=CARTESIAN_POINT('Ctrl Pts',(10.347889599619,-30.6886821199705,1.27216188087579));
#5788=CARTESIAN_POINT('Ctrl Pts',(10.3938110523703,-30.6939867219453,1.31137063355195));
#5789=CARTESIAN_POINT('Ctrl Pts',(10.4412246219906,-30.6985393909015,1.34894683398728));
#5790=CARTESIAN_POINT('Ctrl Pts',(10.4886802733886,-30.7030961005661,1.38655638507146));
#5791=CARTESIAN_POINT('Ctrl Pts',(10.5376300920794,-30.7068994512443,1.42252990566964));
#5792=CARTESIAN_POINT('Ctrl Pts',(10.5878023876643,-30.7099272590381,1.45666435205221));
#5793=CARTESIAN_POINT('Ctrl Pts',(10.637936467929,-30.712952760606,1.49077279885102));
#5794=CARTESIAN_POINT('Ctrl Pts',(10.6892904409665,-30.7152038772653,1.5230445451298));
#5795=CARTESIAN_POINT('Ctrl Pts',(10.7415677450441,-30.7166757718216,1.55331889475982));
#5796=CARTESIAN_POINT('Ctrl Pts',(10.7938152754037,-30.7181468280834,1.58357600210919));
#5797=CARTESIAN_POINT('Ctrl Pts',(10.8469843080727,-30.7188395900405,1.61183773325829));
#5798=CARTESIAN_POINT('Ctrl Pts',(10.9007646124879,-30.7187663790714,1.63799064371833));
#5799=CARTESIAN_POINT('Ctrl Pts',(10.9126652410201,-30.718750178781,1.64377781944754));
#5800=CARTESIAN_POINT('Ctrl Pts',(10.9245957720951,-30.7186965368063,1.6494619246718));
#5801=CARTESIAN_POINT('Ctrl Pts',(10.936552809864,-30.7186056956016,1.65504205590817));
#5802=CARTESIAN_POINT('Ctrl Pts',(10.9905931865086,-30.7181951346406,1.68026171311514));
#5803=CARTESIAN_POINT('Ctrl Pts',(11.0459560513171,-30.7174693653519,1.70359676647102));
#5804=CARTESIAN_POINT('Ctrl Pts',(11.1023631231076,-30.716425003109,1.72487226661216));
#5805=CARTESIAN_POINT('Ctrl Pts',(11.1587898937964,-30.7153802761462,1.74615519674216));
#5806=CARTESIAN_POINT('Ctrl Pts',(11.2162609360083,-30.7140167195368,1.76537666733515));
#5807=CARTESIAN_POINT('Ctrl Pts',(11.2744675877869,-30.7123379996035,1.78240346403925));
#5808=CARTESIAN_POINT('Ctrl Pts',(11.3327259007125,-30.7106577897271,1.79944537282797));
#5809=CARTESIAN_POINT('Ctrl Pts',(11.3917203532232,-30.7086618683655,1.8142883941294));
#5810=CARTESIAN_POINT('Ctrl Pts',(11.4511221884294,-30.7063609989745,1.82684686809454));
#5811=CARTESIAN_POINT('Ctrl Pts',(11.5104787783434,-30.7040618821136,1.83939577649959));
#5812=CARTESIAN_POINT('Ctrl Pts',(11.5702413003453,-30.7014583207647,1.84966349840248));
#5813=CARTESIAN_POINT('Ctrl Pts',(11.6300746296403,-30.6985677421276,1.85761563656223));
#5814=CARTESIAN_POINT('Ctrl Pts',(11.6898738818019,-30.6956788097741,1.86556324570655));
#5815=CARTESIAN_POINT('Ctrl Pts',(11.7497430473299,-30.6925032482214,1.8711979799007));
#5816=CARTESIAN_POINT('Ctrl Pts',(11.809352838627,-30.6890643814319,1.87453687269563));
#5817=CARTESIAN_POINT('Ctrl Pts',(11.8225434293247,-30.6883034211383,1.87527571051545));
#5818=CARTESIAN_POINT('Ctrl Pts',(11.8357213668493,-30.6875295887145,1.87590232633983));
#5819=CARTESIAN_POINT('Ctrl Pts',(11.8488831784818,-30.6867431709956,1.87641723476232));
#5820=CARTESIAN_POINT('Ctrl Pts',(11.9083685854582,-30.6831889203068,1.87874438682333));
#5821=CARTESIAN_POINT('Ctrl Pts',(11.9683565902155,-30.6797928252235,1.87880825693467));
#5822=CARTESIAN_POINT('Ctrl Pts',(12.0285236973258,-30.6765776055765,1.87655505226089));
#5823=CARTESIAN_POINT('Ctrl Pts',(12.0887118164422,-30.6733612630865,1.87430106070617));
#5824=CARTESIAN_POINT('Ctrl Pts',(12.1490783712002,-30.6703259815291,1.86972820122931));
#5825=CARTESIAN_POINT('Ctrl Pts',(12.2092877263483,-30.6674910002661,1.86283322829512));
#5826=CARTESIAN_POINT('Ctrl Pts',(12.2695505201372,-30.6646535028237,1.85593213574744));
#5827=CARTESIAN_POINT('Ctrl Pts',(12.3296549981843,-30.6620167079199,1.84670481534564));
#5828=CARTESIAN_POINT('Ctrl Pts',(12.3892650959708,-30.6595955980721,1.83519995710496));
#5829=CARTESIAN_POINT('Ctrl Pts',(12.4488297898355,-30.6571763323394,1.82370386190449));
#5830=CARTESIAN_POINT('Ctrl Pts',(12.5079000450142,-30.6549724514273,1.80993391118336));
#5831=CARTESIAN_POINT('Ctrl Pts',(12.5661534499491,-30.6529940425448,1.7939888193838));
#5832=CARTESIAN_POINT('Ctrl Pts',(12.6243736775717,-30.651016760434,1.77805280886096));
#5833=CARTESIAN_POINT('Ctrl Pts',(12.6817772619013,-30.64926470285,1.75994451788749));
#5834=CARTESIAN_POINT('Ctrl Pts',(12.7380667732359,-30.6477428005906,1.73980808435039));
#5835=CARTESIAN_POINT('Ctrl Pts',(12.750522644804,-30.6474060305843,1.73535224836905));
#5836=CARTESIAN_POINT('Ctrl Pts',(12.7629240831111,-30.6470805101927,1.73079726584431));
#5837=CARTESIAN_POINT('Ctrl Pts',(12.7752680790299,-30.6467662585964,1.72614496752461));
#5838=CARTESIAN_POINT('Ctrl Pts',(12.8310573306496,-30.6453459841976,1.70511869343341));
#5839=CARTESIAN_POINT('Ctrl Pts',(12.8864681944009,-30.6445925027062,1.68189873004143));
#5840=CARTESIAN_POINT('Ctrl Pts',(12.9411819633194,-30.6445257693322,1.6565630953722));
#5841=CARTESIAN_POINT('Ctrl Pts',(12.9959148397886,-30.6444590126531,1.63121861280354));
#5842=CARTESIAN_POINT('Ctrl Pts',(13.0499493384079,-30.645079545412,1.60375713415863));
#5843=CARTESIAN_POINT('Ctrl Pts',(13.1029743581731,-30.6463924421165,1.57430602553699));
#5844=CARTESIAN_POINT('Ctrl Pts',(13.1560464401424,-30.6477065040787,1.54482877766837));
#5845=CARTESIAN_POINT('Ctrl Pts',(13.2081064812712,-30.6497141669951,1.51335869953463));
#5846=CARTESIAN_POINT('Ctrl Pts',(13.2588623156389,-30.6524050685155,1.48006918736057));
#5847=CARTESIAN_POINT('Ctrl Pts',(13.3095794902154,-30.6550939204255,1.44680503119932));
#5848=CARTESIAN_POINT('Ctrl Pts',(13.3589937747173,-30.6584649167829,1.41172471547181));
#5849=CARTESIAN_POINT('Ctrl Pts',(13.4068442291101,-30.6624926541963,1.3750405146975));
#5850=CARTESIAN_POINT('Ctrl Pts',(13.4546674310278,-30.6665180976751,1.33837720683381));
#5851=CARTESIAN_POINT('Ctrl Pts',(13.5009280586962,-30.6711994291191,1.30011245980355));
#5852=CARTESIAN_POINT('Ctrl Pts',(13.5454051453913,-30.6764974334051,1.26048896755351));
#5853=CARTESIAN_POINT('Ctrl Pts',(13.5552471366691,-30.677669787888,1.25172099073441));
#5854=CARTESIAN_POINT('Ctrl Pts',(13.5650019652857,-30.6788722883136,1.24288658001281));
#5855=CARTESIAN_POINT('Ctrl Pts',(13.5746675343456,-30.6801044271852,1.2339885196899));
#5856=CARTESIAN_POINT('Ctrl Pts',(13.6183515138192,-30.6856731349188,1.19377333090038));
#5857=CARTESIAN_POINT('Ctrl Pts',(13.6608895145213,-30.6923518043743,1.1518685325288));
#5858=CARTESIAN_POINT('Ctrl Pts',(13.7020166722461,-30.7001293046305,1.10846850103127));
#5859=CARTESIAN_POINT('Ctrl Pts',(13.7431581927038,-30.7079095210034,1.06505331305085));
#5860=CARTESIAN_POINT('Ctrl Pts',(13.7828872078749,-30.7167893284822,1.0201422978762));
#5861=CARTESIAN_POINT('Ctrl Pts',(13.820963799237,-30.7267327043492,0.97396820682354));
#5862=CARTESIAN_POINT('Ctrl Pts',(13.8590741853685,-30.736684905431,0.927753134089042));
#5863=CARTESIAN_POINT('Ctrl Pts',(13.8955286265147,-30.7477024656982,0.880273333152889));
#5864=CARTESIAN_POINT('Ctrl Pts',(13.930121366925,-30.7597251338659,0.831792563200548));
#5865=CARTESIAN_POINT('Ctrl Pts',(13.9646877586768,-30.7717386445869,0.783348720164987));
#5866=CARTESIAN_POINT('Ctrl Pts',(13.9973948520632,-30.7847555422319,0.73390612619343));
#5867=CARTESIAN_POINT('Ctrl Pts',(14.0280797616702,-30.7986938115477,0.683748572310606));
#5868=CARTESIAN_POINT('Ctrl Pts',(14.0587471951691,-30.8126241425412,0.633619584874411));
#5869=CARTESIAN_POINT('Ctrl Pts',(14.0873944899397,-30.8274745364751,0.582777184222982));
#5870=CARTESIAN_POINT('Ctrl Pts',(14.1139066028877,-30.84314462319,0.531514551850337));
#5871=CARTESIAN_POINT('Ctrl Pts',(14.1197732637638,-30.8466121357506,0.52017103953455));
#5872=CARTESIAN_POINT('Ctrl Pts',(14.1255355657245,-30.8501197225158,0.508806964006327));
#5873=CARTESIAN_POINT('Ctrl Pts',(14.1311925920689,-30.8536661946033,0.497425511654571));
#5874=CARTESIAN_POINT('Ctrl Pts',(14.1567597802163,-30.8696946366858,0.445986519513703));
#5875=CARTESIAN_POINT('Ctrl Pts',(14.1806788242274,-30.8871229657987,0.39369664540894));
#5876=CARTESIAN_POINT('Ctrl Pts',(14.2027770927318,-30.9058868003686,0.340828125588002));
#5877=CARTESIAN_POINT('Ctrl Pts',(14.2248830785583,-30.9246571877848,0.287941142628218));
#5878=CARTESIAN_POINT('Ctrl Pts',(14.2451665594135,-30.9447638797351,0.234475768277207));
#5879=CARTESIAN_POINT('Ctrl Pts',(14.263491348928,-30.9661109637157,0.180724039815161));
#5880=CARTESIAN_POINT('Ctrl Pts',(14.2818324025568,-30.9874769942394,0.126924604160708));
#5881=CARTESIAN_POINT('Ctrl Pts',(14.2982109611228,-31.0100853707185,0.0728390372992588));
#5882=CARTESIAN_POINT('Ctrl Pts',(14.3125330760228,-31.0338112899811,0.018769220635499));
#5883=CARTESIAN_POINT('Ctrl Pts',(14.3268442820297,-31.0575191376449,-0.0352594120376883));
#5884=CARTESIAN_POINT('Ctrl Pts',(14.3391020279638,-31.0823424715467,-0.0892715721449215));
#5885=CARTESIAN_POINT('Ctrl Pts',(14.349258645209,-31.1081327559841,-0.142968160449075));
#5886=CARTESIAN_POINT('Ctrl Pts',(14.3594094779122,-31.1339083519698,-0.196634166704025));
#5887=CARTESIAN_POINT('Ctrl Pts',(14.367461600142,-31.1606493743139,-0.249984259986138));
#5888=CARTESIAN_POINT('Ctrl Pts',(14.373414373612,-31.1881894012107,-0.302732839444724));
#5889=CARTESIAN_POINT('Ctrl Pts',(14.3747316169147,-31.194283521232,-0.3144051655241));
#5890=CARTESIAN_POINT('Ctrl Pts',(14.3759462441235,-31.2004167092395,-0.326048111329434));
#5891=CARTESIAN_POINT('Ctrl Pts',(14.3770585529418,-31.2065870752141,-0.337658719487507));
#5892=CARTESIAN_POINT('Ctrl Pts',(14.3820856832934,-31.2344743251941,-0.390133391728236));
#5893=CARTESIAN_POINT('Ctrl Pts',(14.3853273896913,-31.2638407207439,-0.442451690706376));
#5894=CARTESIAN_POINT('Ctrl Pts',(14.3867233958332,-31.2945570120615,-0.494317440110226));
#5895=CARTESIAN_POINT('Ctrl Pts',(14.3881198894988,-31.3252840303516,-0.546201302458348));
#5896=CARTESIAN_POINT('Ctrl Pts',(14.3876692117264,-31.3573615943671,-0.59763156288618));
#5897=CARTESIAN_POINT('Ctrl Pts',(14.3853509125449,-31.3906269711632,-0.64831473971449));
#5898=CARTESIAN_POINT('Ctrl Pts',(14.3830305557636,-31.4239218725492,-0.699042900251102));
#5899=CARTESIAN_POINT('Ctrl Pts',(14.3788392239111,-31.4584062807987,-0.749021923205321));
#5900=CARTESIAN_POINT('Ctrl Pts',(14.3727980277331,-31.4938889631939,-0.797971596267801));
#5901=CARTESIAN_POINT('Ctrl Pts',(14.3667614330238,-31.5293446190785,-0.84688398525904));
#5902=CARTESIAN_POINT('Ctrl Pts',(14.3588779192251,-31.5657965147087,-0.894767940776057));
#5903=CARTESIAN_POINT('Ctrl Pts',(14.3492093765965,-31.6030328605358,-0.941368295641471));
#5904=CARTESIAN_POINT('Ctrl Pts',(14.3395463405345,-31.640247998987,-0.987942110006656));
#5905=CARTESIAN_POINT('Ctrl Pts',(14.3281005770856,-31.6782461308766,-1.03323325564961));
#5906=CARTESIAN_POINT('Ctrl Pts',(14.3149716746741,-31.7168029684803,-1.07702027911411));
#5907=CARTESIAN_POINT('Ctrl Pts',(14.3120664811774,-31.7253349135243,-1.08670957162503));
#5908=CARTESIAN_POINT('Ctrl Pts',(14.3090790082963,-31.7338941851498,-1.09632535949905));
#5909=CARTESIAN_POINT('Ctrl Pts',(14.3060105618214,-31.7424783113183,-1.10586550012264));
#5910=CARTESIAN_POINT('Ctrl Pts',(14.2921425782612,-31.7812746604017,-1.14898260006689));
#5911=CARTESIAN_POINT('Ctrl Pts',(14.276743966429,-31.8214030486997,-1.19096704316451));
#5912=CARTESIAN_POINT('Ctrl Pts',(14.2598646740236,-31.8626705885533,-1.23155737439071));
#5913=CARTESIAN_POINT('Ctrl Pts',(14.2429794869057,-31.9039525401653,-1.27216188087552));
#5914=CARTESIAN_POINT('Ctrl Pts',(14.2246126805971,-31.9463739858142,-1.31137063355188));
#5915=CARTESIAN_POINT('Ctrl Pts',(14.204848622758,-31.9897116760678,-1.34894683398738));
#5916=CARTESIAN_POINT('Ctrl Pts',(14.1850670233862,-32.0330878305638,-1.38655638507153));
#5917=CARTESIAN_POINT('Ctrl Pts',(14.1638859123477,-32.0773812923998,-1.42252990566966));
#5918=CARTESIAN_POINT('Ctrl Pts',(14.1414219230224,-32.1223456788394,-1.4566643520522));
#5919=CARTESIAN_POINT('Ctrl Pts',(14.1189750441073,-32.1672758167275,-1.49077279885072));
#5920=CARTESIAN_POINT('Ctrl Pts',(14.0952475818026,-32.2128752202925,-1.52304454512923));
#5921=CARTESIAN_POINT('Ctrl Pts',(14.0703836278415,-32.2588846409427,-1.55331889475902));
#5922=CARTESIAN_POINT('Ctrl Pts',(14.0455338347545,-32.3048678576505,-1.58357600210875));
#5923=CARTESIAN_POINT('Ctrl Pts',(14.0195492678734,-32.3512599716156,-1.61183773325817));
#5924=CARTESIAN_POINT('Ctrl Pts',(13.9925957131064,-32.3977984759783,-1.63799064371848));
#5925=CARTESIAN_POINT('Ctrl Pts',(13.9866313689773,-32.408096622463,-1.64377781944764));
#5926=CARTESIAN_POINT('Ctrl Pts',(13.980619648127,-32.4184019444672,-1.64946192467185));
#5927=CARTESIAN_POINT('Ctrl Pts',(13.9745624584517,-32.4287116223265,-1.65504205590818));
#5928=CARTESIAN_POINT('Ctrl Pts',(13.9471867139074,-32.4753066808503,-1.6802617131151));
#5929=CARTESIAN_POINT('Ctrl Pts',(13.9188767468619,-32.5228894435563,-1.70359676647094));
#5930=CARTESIAN_POINT('Ctrl Pts',(13.8897687667337,-32.5712172195584,-1.72487226661204));
#5931=CARTESIAN_POINT('Ctrl Pts',(13.8606506212992,-32.6195618729473,-1.74615519674216));
#5932=CARTESIAN_POINT('Ctrl Pts',(13.83073422553,-32.6686514771803,-1.76537666733525));
#5933=CARTESIAN_POINT('Ctrl Pts',(13.8001770855324,-32.7182205563234,-1.78240346403942));
#5934=CARTESIAN_POINT('Ctrl Pts',(13.7695928246328,-32.7678336303605,-1.79944537282816));
#5935=CARTESIAN_POINT('Ctrl Pts',(13.7383670797744,-32.8179263642364,-1.81428839412959));
#5936=CARTESIAN_POINT('Ctrl Pts',(13.7066735508278,-32.868219427861,-1.82684686809474));
#5937=CARTESIAN_POINT('Ctrl Pts',(13.6750041622632,-32.9184741841778,-1.83939577649969));
#5938=CARTESIAN_POINT('Ctrl Pts',(13.642868150994,-32.9689282657509,-1.84966349840251));
#5939=CARTESIAN_POINT('Ctrl Pts',(13.6104481718153,-33.0193001595944,-1.85761563656222));
#5940=CARTESIAN_POINT('Ctrl Pts',(13.5780466569263,-33.0696433649174,-1.86556324570659));
#5941=CARTESIAN_POINT('Ctrl Pts',(13.5453619571861,-33.119903802392,-1.87119797990078));
#5942=CARTESIAN_POINT('Ctrl Pts',(13.5125789155374,-33.1698079625751,-1.87453687269571));
#5943=CARTESIAN_POINT('Ctrl Pts',(13.5053246092432,-33.1808508690632,-1.8752757105155));
#5944=CARTESIAN_POINT('Ctrl Pts',(13.4980654819439,-33.1918763815167,-1.87590232633986));
#5945=CARTESIAN_POINT('Ctrl Pts',(13.4908035184053,-33.2028816358906,-1.87641723476233));
#5946=CARTESIAN_POINT('Ctrl Pts',(13.457982743529,-33.2526203841424,-1.87874438682335));
#5947=CARTESIAN_POINT('Ctrl Pts',(13.4250476365344,-33.3028734726432,-1.87880825693469));
#5948=CARTESIAN_POINT('Ctrl Pts',(13.392179621086,-33.3533721060497,-1.87655505226088));
#5949=CARTESIAN_POINT('Ctrl Pts',(13.3593001272239,-33.403888374966,-1.87430106070611));
#5950=CARTESIAN_POINT('Ctrl Pts',(13.3264882189081,-33.4546497041472,-1.86972820122915));
#5951=CARTESIAN_POINT('Ctrl Pts',(13.2939283755408,-33.5053750446201,-1.86283322829481));
#5952=CARTESIAN_POINT('Ctrl Pts',(13.261339633778,-33.5561454062231,-1.85593213574705));
#5953=CARTESIAN_POINT('Ctrl Pts',(13.2290038633833,-33.6068790136412,-1.84670481534519));
#5954=CARTESIAN_POINT('Ctrl Pts',(13.1971020718565,-33.6572923177224,-1.83519995710444));
#5955=CARTESIAN_POINT('Ctrl Pts',(13.1652245793415,-33.7076672229108,-1.82370386190406));
#5956=CARTESIAN_POINT('Ctrl Pts',(13.1337808348958,-33.7577216240468,-1.8099339111831));
#5957=CARTESIAN_POINT('Ctrl Pts',(13.1029407800775,-33.8071813481355,-1.79398881938374));
#5958=CARTESIAN_POINT('Ctrl Pts',(13.0721182897278,-33.8566129032153,-1.77805280886091));
#5959=CARTESIAN_POINT('Ctrl Pts',(13.0418991711865,-33.905449836721,-1.75994451788745));
#5960=CARTESIAN_POINT('Ctrl Pts',(13.0124364095004,-33.9534370323736,-1.73980808435037));
#5961=CARTESIAN_POINT('Ctrl Pts',(13.0059168223358,-33.9640557485747,-1.73535224836903));
#5962=CARTESIAN_POINT('Ctrl Pts',(12.9994341942536,-33.9746329489963,-1.7307972658443));
#5963=CARTESIAN_POINT('Ctrl Pts',(12.9929900464286,-33.9851660372479,-1.72614496752461));
#5964=CARTESIAN_POINT('Ctrl Pts',(12.9638654269088,-34.0327708092098,-1.70511869343321));
#5965=CARTESIAN_POINT('Ctrl Pts',(12.9355074609201,-34.0803812841189,-1.68189873004098));
#5966=CARTESIAN_POINT('Ctrl Pts',(12.9080927836634,-34.1277314312526,-1.65656309537146));
#5967=CARTESIAN_POINT('Ctrl Pts',(12.8806685324485,-34.1750981143581,-1.63121861280245));
#5968=CARTESIAN_POINT('Ctrl Pts',(12.8541886802717,-34.2222036292231,-1.60375713415714));
#5969=CARTESIAN_POINT('Ctrl Pts',(12.8288131722874,-34.2687810917287,-1.57430602553505));
#5970=CARTESIAN_POINT('Ctrl Pts',(12.8034151423441,-34.3153998939271,-1.54482877766629));
#5971=CARTESIAN_POINT('Ctrl Pts',(12.7791238088676,-34.3614890435249,-1.51335869953241));
#5972=CARTESIAN_POINT('Ctrl Pts',(12.7560762807596,-34.4067903362379,-1.48006918735819));
#5973=CARTESIAN_POINT('Ctrl Pts',(12.7330463075327,-34.4520571237836,-1.44680503119733));
#5974=CARTESIAN_POINT('Ctrl Pts',(12.7112585337638,-34.4965366476502,-1.41172471547026));
#5975=CARTESIAN_POINT('Ctrl Pts',(12.6908214294875,-34.539990225443,-1.37504051469644));
#5976=CARTESIAN_POINT('Ctrl Pts',(12.6703959648427,-34.5834190549336,-1.33837720683257));
#5977=CARTESIAN_POINT('Ctrl Pts',(12.6513198029624,-34.6258225994116,-1.30011245980211));
#5978=CARTESIAN_POINT('Ctrl Pts',(12.6336694659159,-34.666989888519,-1.26048896755186));
#5979=CARTESIAN_POINT('Ctrl Pts',(12.6297637590416,-34.6760994802303,-1.2517209907333));
#5980=CARTESIAN_POINT('Ctrl Pts',(12.6259277406503,-34.6851486598341,-1.24288658001226));
#5981=CARTESIAN_POINT('Ctrl Pts',(12.6221620196843,-34.6941353576172,-1.23398851968991));
#5982=CARTESIAN_POINT('Ctrl Pts',(12.6051426723111,-34.7347511474464,-1.19377333090049));
#5983=CARTESIAN_POINT('Ctrl Pts',(12.589657569372,-34.7749294714083,-1.15186853252901));
#5984=CARTESIAN_POINT('Ctrl Pts',(12.5758295033095,-34.8144353849114,-1.10846850103161));
#5985=CARTESIAN_POINT('Ctrl Pts',(12.5619966081066,-34.8539550949644,-1.06505331305148));
#5986=CARTESIAN_POINT('Ctrl Pts',(12.5498222393785,-34.8928013351089,-1.02014229787715));
#5987=CARTESIAN_POINT('Ctrl Pts',(12.5393951597977,-34.9307483184514,-0.973968206824812));
#5988=CARTESIAN_POINT('Ctrl Pts',(12.5289588256923,-34.9687289815301,-0.927753134090402));
#5989=CARTESIAN_POINT('Ctrl Pts',(12.5202730921983,-35.0058082337771,-0.88027333315432));
#5990=CARTESIAN_POINT('Ctrl Pts',(12.5133886580476,-35.0417777598427,-0.831792563202067));
#5991=CARTESIAN_POINT('Ctrl Pts',(12.5065094676445,-35.0777198885782,-0.783348720165615));
#5992=CARTESIAN_POINT('Ctrl Pts',(12.5014288849903,-35.1125535111578,-0.733906126193128));
#5993=CARTESIAN_POINT('Ctrl Pts',(12.498157325499,-35.1460965570489,-0.683748572309347));
#5994=CARTESIAN_POINT('Ctrl Pts',(12.4948876292731,-35.1796204990247,-0.633619584872897));
#5995=CARTESIAN_POINT('Ctrl Pts',(12.4934248002908,-35.2118549810128,-0.582777184221212));
#5996=CARTESIAN_POINT('Ctrl Pts',(12.4937394369914,-35.2426501876914,-0.531514551848308));
#5997=CARTESIAN_POINT('Ctrl Pts',(12.4938090605188,-35.2494646213253,-0.520171039533193));
#5998=CARTESIAN_POINT('Ctrl Pts',(12.4939655687831,-35.2562087145898,-0.508806964005651));
#5999=CARTESIAN_POINT('Ctrl Pts',(12.4942083905325,-35.2628810791572,-0.497425511654571));
#6000=CARTESIAN_POINT('Ctrl Pts',(12.4953058344853,-35.2930371346372,-0.445986519514037));
#6001=CARTESIAN_POINT('Ctrl Pts',(12.4984396882371,-35.3224657989414,-0.393696645409609));
#6002=CARTESIAN_POINT('Ctrl Pts',(12.5036405113948,-35.3509853781306,-0.340828125589025));
#6003=CARTESIAN_POINT('Ctrl Pts',(12.5088431508228,-35.3795149171403,-0.287941142629085));
#6004=CARTESIAN_POINT('Ctrl Pts',(12.5161143164102,-35.4071342728133,-0.234475768277919));
#6005=CARTESIAN_POINT('Ctrl Pts',(12.5254390386769,-35.4336775480422,-0.180724039815708));
#6006=CARTESIAN_POINT('Ctrl Pts',(12.5347720370741,-35.460244381679,-0.126924604161013));
#6007=CARTESIAN_POINT('Ctrl Pts',(12.5461621861603,-35.4857328177141,-0.0728390372993232));
#6008=CARTESIAN_POINT('Ctrl Pts',(12.55954837752,-35.5099990926848,-0.0187692206353172));
#6009=CARTESIAN_POINT('Ctrl Pts',(12.5729243728623,-35.5342468844775,0.035259412037625));
#6010=CARTESIAN_POINT('Ctrl Pts',(12.5882931376608,-35.5572740708003,0.0892715721446082));
#6011=CARTESIAN_POINT('Ctrl Pts',(12.6055498705317,-35.5789651015697,0.142968160448519));
#6012=CARTESIAN_POINT('Ctrl Pts',(12.6227967751013,-35.6006437785531,0.196634166703384));
#6013=CARTESIAN_POINT('Ctrl Pts',(12.6419291186596,-35.6209876321305,0.249984259985418));
#6014=CARTESIAN_POINT('Ctrl Pts',(12.662803094838,-35.6399128986269,0.302732839443923));
#6015=CARTESIAN_POINT('Ctrl Pts',(12.6674221359389,-35.6441007248007,0.314405165523565));
#6016=CARTESIAN_POINT('Ctrl Pts',(12.6721263189554,-35.6482192168235,0.326048111329166));
#6017=CARTESIAN_POINT('Ctrl Pts',(12.676913858231,-35.6522676875044,0.337658719487503));
#6018=CARTESIAN_POINT('Ctrl Pts',(12.6985513599797,-35.6705649350872,0.390133391728747));
#6019=CARTESIAN_POINT('Ctrl Pts',(12.7223625513447,-35.6880555329546,0.4424516907074));
#6020=CARTESIAN_POINT('Ctrl Pts',(12.7482656368651,-35.7046226553962,0.49431744011175));
#6021=CARTESIAN_POINT('Ctrl Pts',(12.7741777684545,-35.7211955635321,0.546201302460495));
#6022=CARTESIAN_POINT('Ctrl Pts',(12.80218309267,-35.7368440471401,0.597631562888927));
#6023=CARTESIAN_POINT('Ctrl Pts',(12.8321509036332,-35.7514690295535,0.648314739717827));
#6024=CARTESIAN_POINT('Ctrl Pts',(12.8621453124406,-35.766106992328,0.699042900254311));
#6025=CARTESIAN_POINT('Ctrl Pts',(12.8941053519454,-35.7797193965928,0.749021923208405));
#6026=CARTESIAN_POINT('Ctrl Pts',(12.9278548543831,-35.7922289084309,0.797971596270746));
#6027=CARTESIAN_POINT('Ctrl Pts',(12.9615786504418,-35.8047288920026,0.846883985262079));
#6028=CARTESIAN_POINT('Ctrl Pts',(12.9970886749731,-35.8161275165969,0.89476794077918));
#6029=CARTESIAN_POINT('Ctrl Pts',(13.034170567718,-35.8263724859765,0.941368295644665));
#6030=CARTESIAN_POINT('Ctrl Pts',(13.0712313410528,-35.8366116204946,0.987942110009404));
#6031=CARTESIAN_POINT('Ctrl Pts',(13.1098615702898,-35.8456983645268,1.03323325565192));
#6032=CARTESIAN_POINT('Ctrl Pts',(13.1498172223497,-35.8536068203165,1.077020279116));
#6033=CARTESIAN_POINT('Ctrl Pts',(13.1586587002493,-35.8553568214672,1.08670957162628));
#6034=CARTESIAN_POINT('Ctrl Pts',(13.1675649833548,-35.8570492298717,1.09632535949967));
#6035=CARTESIAN_POINT('Ctrl Pts',(13.1765332779228,-35.8586839403584,1.10586550012264));
#6036=CARTESIAN_POINT('Ctrl Pts',(13.2170658935831,-35.8660720888377,1.14898260006675));
#6037=CARTESIAN_POINT('Ctrl Pts',(13.2595174031781,-35.872800693957,1.19096704316422));
#6038=CARTESIAN_POINT('Ctrl Pts',(13.3036957872455,-35.8788165678628,1.23155737439029));
#6039=CARTESIAN_POINT('Ctrl Pts',(13.3478895996175,-35.8848345426769,1.27216188087445));
#6040=CARTESIAN_POINT('Ctrl Pts',(13.3938110523682,-35.8901391446517,1.31137063355021));
#6041=CARTESIAN_POINT('Ctrl Pts',(13.4412246219879,-35.8946918136079,1.34894683398517));
#6042=CARTESIAN_POINT('Ctrl Pts',(13.4886802733859,-35.8992485232725,1.38655638506951));
#6043=CARTESIAN_POINT('Ctrl Pts',(13.5376300920768,-35.9030518739508,1.42252990566782));
#6044=CARTESIAN_POINT('Ctrl Pts',(13.5878023876618,-35.9060796817446,1.45666435205053));
#6045=CARTESIAN_POINT('Ctrl Pts',(13.6379364679262,-35.9091051833125,1.49077279884923));
#6046=CARTESIAN_POINT('Ctrl Pts',(13.6892904409634,-35.9113562999719,1.52304454512792));
#6047=CARTESIAN_POINT('Ctrl Pts',(13.7415677450407,-35.9128281945281,1.55331889475788));
#6048=CARTESIAN_POINT('Ctrl Pts',(13.7938152754001,-35.91429925079,1.58357600210724));
#6049=CARTESIAN_POINT('Ctrl Pts',(13.8469843080689,-35.9149920127471,1.61183773325636));
#6050=CARTESIAN_POINT('Ctrl Pts',(13.9007646124839,-35.914918801778,1.63799064371642));
#6051=CARTESIAN_POINT('Ctrl Pts',(13.9126652410174,-35.9149026014877,1.64377781944629));
#6052=CARTESIAN_POINT('Ctrl Pts',(13.9245957720938,-35.914848959513,1.64946192467119));
#6053=CARTESIAN_POINT('Ctrl Pts',(13.9365528098639,-35.9147581183082,1.65504205590817));
#6054=CARTESIAN_POINT('Ctrl Pts',(13.9905931865086,-35.9143475573472,1.68026171311514));
#6055=CARTESIAN_POINT('Ctrl Pts',(14.0459560513171,-35.9136217880585,1.70359676647103));
#6056=CARTESIAN_POINT('Ctrl Pts',(14.1023631231076,-35.9125774258157,1.72487226661217));
#6057=CARTESIAN_POINT('Ctrl Pts',(14.1587898937969,-35.9115326988529,1.74615519674234));
#6058=CARTESIAN_POINT('Ctrl Pts',(14.2162609360092,-35.9101691422435,1.76537666733546));
#6059=CARTESIAN_POINT('Ctrl Pts',(14.2744675877883,-35.9084904223101,1.78240346403966));
#6060=CARTESIAN_POINT('Ctrl Pts',(14.3327259007139,-35.9068102124337,1.79944537282833));
#6061=CARTESIAN_POINT('Ctrl Pts',(14.3917203532245,-35.9048142910721,1.81428839412971));
#6062=CARTESIAN_POINT('Ctrl Pts',(14.4511221884307,-35.9025134216811,1.82684686809481));
#6063=CARTESIAN_POINT('Ctrl Pts',(14.5104787783442,-35.9002143048202,1.83939577649974));
#6064=CARTESIAN_POINT('Ctrl Pts',(14.5702413003456,-35.8976107434714,1.84966349840254));
#6065=CARTESIAN_POINT('Ctrl Pts',(14.6300746296402,-35.8947201648342,1.85761563656223));
#6066=CARTESIAN_POINT('Ctrl Pts',(14.6898738818023,-35.8918312324807,1.8655632457066));
#6067=CARTESIAN_POINT('Ctrl Pts',(14.7497430473307,-35.888655670928,1.87119797990078));
#6068=CARTESIAN_POINT('Ctrl Pts',(14.8093528386281,-35.8852168041384,1.8745368726957));
#6069=CARTESIAN_POINT('Ctrl Pts',(14.8225434293255,-35.8844558438449,1.87527571051549));
#6070=CARTESIAN_POINT('Ctrl Pts',(14.8357213668496,-35.8836820114211,1.87590232633985));
#6071=CARTESIAN_POINT('Ctrl Pts',(14.8488831784817,-35.8828955937023,1.87641723476232));
#6072=CARTESIAN_POINT('Ctrl Pts',(14.9083685854582,-35.8793413430134,1.87874438682333));
#6073=CARTESIAN_POINT('Ctrl Pts',(14.9683565902156,-35.8759452479302,1.87880825693468));
#6074=CARTESIAN_POINT('Ctrl Pts',(15.0285236973261,-35.8727300282831,1.87655505226089));
#6075=CARTESIAN_POINT('Ctrl Pts',(15.0887118164435,-35.8695136857931,1.87430106070612));
#6076=CARTESIAN_POINT('Ctrl Pts',(15.1490783712027,-35.8664784042356,1.86972820122912));
#6077=CARTESIAN_POINT('Ctrl Pts',(15.209287726352,-35.8636434229726,1.8628332282947));
#6078=CARTESIAN_POINT('Ctrl Pts',(15.2695505201408,-35.8608059255302,1.85593213574694));
#6079=CARTESIAN_POINT('Ctrl Pts',(15.3296549981877,-35.8581691306264,1.84670481534507));
#6080=CARTESIAN_POINT('Ctrl Pts',(15.3892650959741,-35.8557480207786,1.83519995710432));
#6081=CARTESIAN_POINT('Ctrl Pts',(15.4488297898389,-35.8533287550459,1.82370386190375));
#6082=CARTESIAN_POINT('Ctrl Pts',(15.5079000450177,-35.8511248741338,1.80993391118252));
#6083=CARTESIAN_POINT('Ctrl Pts',(15.5661534499527,-35.8491464652513,1.79398881938283));
#6084=CARTESIAN_POINT('Ctrl Pts',(15.6243736775756,-35.8471691831405,1.77805280885979));
#6085=CARTESIAN_POINT('Ctrl Pts',(15.6817772619055,-35.8454171255565,1.7599445178861));
#6086=CARTESIAN_POINT('Ctrl Pts',(15.7380667732405,-35.8438952232971,1.73980808434875));
#6087=CARTESIAN_POINT('Ctrl Pts',(15.750522644807,-35.8435584532909,1.73535224836793));
#6088=CARTESIAN_POINT('Ctrl Pts',(15.7629240831126,-35.8432329328993,1.73079726584374));
#6089=CARTESIAN_POINT('Ctrl Pts',(15.7752680790298,-35.842918681303,1.72614496752462));
#6090=CARTESIAN_POINT('Ctrl Pts',(15.8310573306496,-35.8414984069043,1.70511869343338));
#6091=CARTESIAN_POINT('Ctrl Pts',(15.8864681944011,-35.8407449254129,1.68189873004136));
#6092=CARTESIAN_POINT('Ctrl Pts',(15.9411819633197,-35.8406781920389,1.65656309537207));
#6093=CARTESIAN_POINT('Ctrl Pts',(15.9959148397889,-35.8406114353597,1.6312186128034));
#6094=CARTESIAN_POINT('Ctrl Pts',(16.0499493384081,-35.8412319681187,1.60375713415847));
#6095=CARTESIAN_POINT('Ctrl Pts',(16.1029743581733,-35.8425448648231,1.57430602553681));
#6096=CARTESIAN_POINT('Ctrl Pts',(16.1560464401428,-35.8438589267853,1.54482877766814));
#6097=CARTESIAN_POINT('Ctrl Pts',(16.2081064812716,-35.8458665897017,1.51335869953437));
#6098=CARTESIAN_POINT('Ctrl Pts',(16.2588623156393,-35.8485574912222,1.48006918736026));
#6099=CARTESIAN_POINT('Ctrl Pts',(16.3095794902158,-35.8512463431322,1.44680503119899));
#6100=CARTESIAN_POINT('Ctrl Pts',(16.3589937747177,-35.8546173394896,1.41172471547146));
#6101=CARTESIAN_POINT('Ctrl Pts',(16.4068442291105,-35.858645076903,1.37504051469712));
#6102=CARTESIAN_POINT('Ctrl Pts',(16.4546674310271,-35.8626705203817,1.33837720683427));
#6103=CARTESIAN_POINT('Ctrl Pts',(16.5009280586945,-35.8673518518255,1.30011245980493));
#6104=CARTESIAN_POINT('Ctrl Pts',(16.5454051453886,-35.8726498561114,1.26048896755585));
#6105=CARTESIAN_POINT('Ctrl Pts',(16.5552471366674,-35.8738222105944,1.25172099073598));
#6106=CARTESIAN_POINT('Ctrl Pts',(16.5650019652848,-35.8750247110202,1.24288658001361));
#6107=CARTESIAN_POINT('Ctrl Pts',(16.5746675343456,-35.8762568498918,1.2339885196899));
#6108=CARTESIAN_POINT('Ctrl Pts',(16.6183515138188,-35.8818255576253,1.19377333090077));
#6109=CARTESIAN_POINT('Ctrl Pts',(16.6608895145205,-35.8885042270808,1.15186853252961));
#6110=CARTESIAN_POINT('Ctrl Pts',(16.7020166722449,-35.8962817273369,1.10846850103254));
#6111=CARTESIAN_POINT('Ctrl Pts',(16.7431581927026,-35.9040619437098,1.06505331305215));
#6112=CARTESIAN_POINT('Ctrl Pts',(16.7828872078737,-35.9129417511886,1.02014229787755));
#6113=CARTESIAN_POINT('Ctrl Pts',(16.8209637992359,-35.9228851270556,0.973968206824924));
#6114=CARTESIAN_POINT('Ctrl Pts',(16.8590741853672,-35.9328373281373,0.927753134090565));
#6115=CARTESIAN_POINT('Ctrl Pts',(16.8955286265134,-35.9438548884045,0.880273333154538));
#6116=CARTESIAN_POINT('Ctrl Pts',(16.9301213669236,-35.9558775565721,0.831792563202344));
#6117=CARTESIAN_POINT('Ctrl Pts',(16.9646877586765,-35.9678910672934,0.783348720165493));
#6118=CARTESIAN_POINT('Ctrl Pts',(16.9973948520637,-35.9809079649387,0.733906126192583));
#6119=CARTESIAN_POINT('Ctrl Pts',(17.0280797616715,-35.9948462342549,0.683748572308376));
#6120=CARTESIAN_POINT('Ctrl Pts',(17.0587471951712,-36.0087765652489,0.633619584870814));
#6121=CARTESIAN_POINT('Ctrl Pts',(17.0873944899424,-36.0236269591832,0.582777184217972));
#6122=CARTESIAN_POINT('Ctrl Pts',(17.113906602891,-36.0392970458986,0.531514551843913));
#6123=CARTESIAN_POINT('Ctrl Pts',(17.1197732637659,-36.0427645584586,0.520171039530256));
#6124=CARTESIAN_POINT('Ctrl Pts',(17.1255355657255,-36.0462721452231,0.508806964004177));
#6125=CARTESIAN_POINT('Ctrl Pts',(17.1311925920688,-36.0498186173099,0.497425511654565));
#6126=CARTESIAN_POINT('Ctrl Pts',(17.1567597802163,-36.0658470593925,0.445986519513662));
#6127=CARTESIAN_POINT('Ctrl Pts',(17.1806788242274,-36.0832753885054,0.393696645408846));
#6128=CARTESIAN_POINT('Ctrl Pts',(17.2027770927318,-36.1020392230754,0.340828125587867));
#6129=CARTESIAN_POINT('Ctrl Pts',(17.2248830785582,-36.1208096104915,0.287941142628222));
#6130=CARTESIAN_POINT('Ctrl Pts',(17.2451665594134,-36.1409163024417,0.234475768277352));
#6131=CARTESIAN_POINT('Ctrl Pts',(17.2634913489279,-36.1622633864223,0.180724039815448));
#6132=CARTESIAN_POINT('Ctrl Pts',(17.2818324025569,-36.1836294169462,0.126924604160518));
#6133=CARTESIAN_POINT('Ctrl Pts',(17.2982109611229,-36.2062377934255,0.0728390372985996));
#6134=CARTESIAN_POINT('Ctrl Pts',(17.312533076023,-36.2299637126883,0.0187692206343586));
#6135=CARTESIAN_POINT('Ctrl Pts',(17.32684428203,-36.2536715603521,-0.035259412038812));
#6136=CARTESIAN_POINT('Ctrl Pts',(17.339102027964,-36.2784948942539,-0.0892715721460276));
#6137=CARTESIAN_POINT('Ctrl Pts',(17.3492586452091,-36.3042851786913,-0.142968160450158));
#6138=CARTESIAN_POINT('Ctrl Pts',(17.3594094779124,-36.3300607746771,-0.19663416670548));
#6139=CARTESIAN_POINT('Ctrl Pts',(17.3674616001422,-36.3568017970215,-0.249984259987957));
#6140=CARTESIAN_POINT('Ctrl Pts',(17.3734143736122,-36.3843418239185,-0.302732839446895));
#6141=CARTESIAN_POINT('Ctrl Pts',(17.3747316169148,-36.3904359439394,-0.314405165525541));
#6142=CARTESIAN_POINT('Ctrl Pts',(17.3759462441235,-36.3965691319466,-0.326048111330149));
#6143=CARTESIAN_POINT('Ctrl Pts',(17.3770585529417,-36.4027394979208,-0.3376587194875));
#6144=CARTESIAN_POINT('Ctrl Pts',(17.3820856832934,-36.4306267479012,-0.390133391729108));
#6145=CARTESIAN_POINT('Ctrl Pts',(17.3853273896914,-36.4599931434515,-0.442451690708116));
#6146=CARTESIAN_POINT('Ctrl Pts',(17.3867233958333,-36.4907094347696,-0.49431744011282));
#6147=CARTESIAN_POINT('Ctrl Pts',(17.3881198894988,-36.5214364530601,-0.546201302461415));
#6148=CARTESIAN_POINT('Ctrl Pts',(17.3876692117263,-36.553514017076,-0.597631562889711));
#6149=CARTESIAN_POINT('Ctrl Pts',(17.3853509125446,-36.5867793938725,-0.648314739718458));
#6150=CARTESIAN_POINT('Ctrl Pts',(17.3830305557632,-36.6200742952585,-0.699042900255015));
#6151=CARTESIAN_POINT('Ctrl Pts',(17.3788392239107,-36.654558703508,-0.749021923209178));
#6152=CARTESIAN_POINT('Ctrl Pts',(17.3727980277326,-36.6900413859033,-0.797971596271591));
#6153=CARTESIAN_POINT('Ctrl Pts',(17.3667614330232,-36.7254970417877,-0.846883985262451));
#6154=CARTESIAN_POINT('Ctrl Pts',(17.3588779192245,-36.7619489374177,-0.894767940779093));
#6155=CARTESIAN_POINT('Ctrl Pts',(17.3492093765959,-36.7991852832446,-0.941368295644146));
#6156=CARTESIAN_POINT('Ctrl Pts',(17.3395463405339,-36.8364004216957,-0.987942110009194));
#6157=CARTESIAN_POINT('Ctrl Pts',(17.3281005770849,-36.8743985535853,-1.03323325565201));
#6158=CARTESIAN_POINT('Ctrl Pts',(17.3149716746734,-36.912955391189,-1.07702027911637));
#6159=CARTESIAN_POINT('Ctrl Pts',(17.3120664811769,-36.9214873362323,-1.08670957162653));
#6160=CARTESIAN_POINT('Ctrl Pts',(17.309079008296,-36.9300466078572,-1.09632535949979));
#6161=CARTESIAN_POINT('Ctrl Pts',(17.3060105618214,-36.9386307340249,-1.10586550012263));
#6162=CARTESIAN_POINT('Ctrl Pts',(17.2921425782612,-36.9774270831083,-1.14898260006685));
#6163=CARTESIAN_POINT('Ctrl Pts',(17.276743966429,-37.0175554714064,-1.19096704316446));
#6164=CARTESIAN_POINT('Ctrl Pts',(17.2598646740236,-37.0588230112599,-1.23155737439063));
#6165=CARTESIAN_POINT('Ctrl Pts',(17.2429794869056,-37.1001049628722,-1.27216188087575));
#6166=CARTESIAN_POINT('Ctrl Pts',(17.2246126805968,-37.1425264085214,-1.31137063355239));
#6167=CARTESIAN_POINT('Ctrl Pts',(17.2048486227575,-37.1858640987754,-1.34894683398816));
#6168=CARTESIAN_POINT('Ctrl Pts',(17.1850670233857,-37.2292402532715,-1.38655638507238));
#6169=CARTESIAN_POINT('Ctrl Pts',(17.1638859123471,-37.2735337151076,-1.42252990567058));
#6170=CARTESIAN_POINT('Ctrl Pts',(17.1414219230217,-37.3184981015473,-1.45666435205317));
#6171=CARTESIAN_POINT('Ctrl Pts',(17.1189750441068,-37.363428239435,-1.49077279885125));
#6172=CARTESIAN_POINT('Ctrl Pts',(17.0952475818025,-37.4090276429994,-1.52304454512938));
#6173=CARTESIAN_POINT('Ctrl Pts',(17.0703836278416,-37.4550370636491,-1.55331889475882));
#6174=CARTESIAN_POINT('Ctrl Pts',(17.0455338347552,-37.5010202803558,-1.58357600210788));
#6175=CARTESIAN_POINT('Ctrl Pts',(17.0195492678746,-37.5474123943199,-1.61183773325672));
#6176=CARTESIAN_POINT('Ctrl Pts',(16.9925957131083,-37.5939508986816,-1.63799064371655));
#6177=CARTESIAN_POINT('Ctrl Pts',(16.9866313689786,-37.6042490451674,-1.64377781944638));
#6178=CARTESIAN_POINT('Ctrl Pts',(16.9806196481277,-37.6145543671727,-1.64946192467123));
#6179=CARTESIAN_POINT('Ctrl Pts',(16.9745624584517,-37.6248640450332,-1.65504205590818));
#6180=CARTESIAN_POINT('Ctrl Pts',(16.9471867139075,-37.6714591035566,-1.68026171311492));
#6181=CARTESIAN_POINT('Ctrl Pts',(16.9188767468623,-37.7190418662623,-1.70359676647061));
#6182=CARTESIAN_POINT('Ctrl Pts',(16.8897687667342,-37.767369642264,-1.72487226661159));
#6183=CARTESIAN_POINT('Ctrl Pts',(16.8606506213001,-37.8157142956525,-1.74615519674153));
#6184=CARTESIAN_POINT('Ctrl Pts',(16.8307342255311,-37.8648038998849,-1.76537666733448));
#6185=CARTESIAN_POINT('Ctrl Pts',(16.8001770855338,-37.9143729790276,-1.78240346403856));
#6186=CARTESIAN_POINT('Ctrl Pts',(16.7695928246345,-37.9639860530644,-1.79944537282729));
#6187=CARTESIAN_POINT('Ctrl Pts',(16.7383670797762,-38.0140787869401,-1.81428839412874));
#6188=CARTESIAN_POINT('Ctrl Pts',(16.7066735508298,-38.0643718505644,-1.82684686809392));
#6189=CARTESIAN_POINT('Ctrl Pts',(16.6750041622648,-38.1146266068819,-1.83939577649913));
#6190=CARTESIAN_POINT('Ctrl Pts',(16.6428681509952,-38.1650806884555,-1.84966349840215));
#6191=CARTESIAN_POINT('Ctrl Pts',(16.6104481718161,-38.2154525822997,-1.857615636562));
#6192=CARTESIAN_POINT('Ctrl Pts',(16.5780466569275,-38.2657957876221,-1.86556324570632));
#6193=CARTESIAN_POINT('Ctrl Pts',(16.5453619571878,-38.3160562250962,-1.8711979799005));
#6194=CARTESIAN_POINT('Ctrl Pts',(16.5125789155394,-38.3659603852787,-1.87453687269548));
#6195=CARTESIAN_POINT('Ctrl Pts',(16.5053246092446,-38.3770032917678,-1.87527571051537));
#6196=CARTESIAN_POINT('Ctrl Pts',(16.4980654819446,-38.3880288042224,-1.8759023263398));
#6197=CARTESIAN_POINT('Ctrl Pts',(16.4908035184053,-38.3990340585972,-1.87641723476232));
#6198=CARTESIAN_POINT('Ctrl Pts',(16.4579827435291,-38.4487728068489,-1.87874438682333));
#6199=CARTESIAN_POINT('Ctrl Pts',(16.4250476365346,-38.4990258953495,-1.87880825693467));
#6200=CARTESIAN_POINT('Ctrl Pts',(16.3921796210864,-38.5495245287558,-1.87655505226089));
#6201=CARTESIAN_POINT('Ctrl Pts',(16.3593001272248,-38.6000407976712,-1.87430106070618));
#6202=CARTESIAN_POINT('Ctrl Pts',(16.3264882189097,-38.6508021268515,-1.86972820122937));
#6203=CARTESIAN_POINT('Ctrl Pts',(16.2939283755429,-38.7015274673234,-1.86283322829525));
#6204=CARTESIAN_POINT('Ctrl Pts',(16.2613396337801,-38.7522978289265,-1.85593213574759));
#6205=CARTESIAN_POINT('Ctrl Pts',(16.2290038633852,-38.8030314363447,-1.8467048153458));
#6206=CARTESIAN_POINT('Ctrl Pts',(16.1971020718583,-38.853444740426,-1.83519995710512));
#6207=CARTESIAN_POINT('Ctrl Pts',(16.1652245793432,-38.9038196456148,-1.82370386190477));
#6208=CARTESIAN_POINT('Ctrl Pts',(16.1337808348973,-38.9538740467511,-1.8099339111838));
#6209=CARTESIAN_POINT('Ctrl Pts',(16.1029407800788,-39.00333377084,-1.79398881938442));
#6210=CARTESIAN_POINT('Ctrl Pts',(16.072118289729,-39.0527653259201,-1.77805280886157));
#6211=CARTESIAN_POINT('Ctrl Pts',(16.0418991711874,-39.101602259426,-1.75994451788808));
#6212=CARTESIAN_POINT('Ctrl Pts',(16.0124364095012,-39.1495894550789,-1.73980808435094));
#6213=CARTESIAN_POINT('Ctrl Pts',(16.0059168223363,-39.1602081712804,-1.73535224836942));
#6214=CARTESIAN_POINT('Ctrl Pts',(15.9994341942539,-39.1707853717025,-1.7307972658445));
#6215=CARTESIAN_POINT('Ctrl Pts',(15.9929900464286,-39.1813184599546,-1.72614496752462));
#6216=CARTESIAN_POINT('Ctrl Pts',(15.963865426909,-39.2289232319161,-1.70511869343336));
#6217=CARTESIAN_POINT('Ctrl Pts',(15.9355074609204,-39.2765337068249,-1.68189873004132));
#6218=CARTESIAN_POINT('Ctrl Pts',(15.908092783664,-39.3238838539582,-1.65656309537201));
#6219=CARTESIAN_POINT('Ctrl Pts',(15.8806685324492,-39.3712505370635,-1.63121861280318));
#6220=CARTESIAN_POINT('Ctrl Pts',(15.8541886802725,-39.4183560519282,-1.60375713415806));
#6221=CARTESIAN_POINT('Ctrl Pts',(15.8288131722884,-39.4649335144336,-1.57430602553619));
#6222=CARTESIAN_POINT('Ctrl Pts',(15.8034151423452,-39.5115523166318,-1.54482877766759));
#6223=CARTESIAN_POINT('Ctrl Pts',(15.7791238088687,-39.5576414662295,-1.51335869953388));
#6224=CARTESIAN_POINT('Ctrl Pts',(15.7560762807607,-39.6029427589422,-1.48006918735986));
#6225=CARTESIAN_POINT('Ctrl Pts',(15.7330463075338,-39.6482095464881,-1.44680503119899));
#6226=CARTESIAN_POINT('Ctrl Pts',(15.7112585337647,-39.6926890703548,-1.41172471547191));
#6227=CARTESIAN_POINT('Ctrl Pts',(15.6908214294883,-39.7361426481477,-1.37504051469807));
#6228=CARTESIAN_POINT('Ctrl Pts',(15.6703959648435,-39.7795714776383,-1.33837720683433));
#6229=CARTESIAN_POINT('Ctrl Pts',(15.6513198029633,-39.8219750221162,-1.300112459804));
#6230=CARTESIAN_POINT('Ctrl Pts',(15.6336694659168,-39.8631423112235,-1.26048896755389));
#6231=CARTESIAN_POINT('Ctrl Pts',(15.6297637590422,-39.8722519029356,-1.25172099073466));
#6232=CARTESIAN_POINT('Ctrl Pts',(15.6259277406505,-39.8813010825401,-1.24288658001294));
#6233=CARTESIAN_POINT('Ctrl Pts',(15.6221620196843,-39.8902877803239,-1.23398851968989));
#6234=CARTESIAN_POINT('Ctrl Pts',(15.6051426723112,-39.9309035701529,-1.1937733309007));
#6235=CARTESIAN_POINT('Ctrl Pts',(15.5896575693722,-39.9710818941145,-1.15186853252947));
#6236=CARTESIAN_POINT('Ctrl Pts',(15.5758295033097,-40.0105878076174,-1.10846850103232));
#6237=CARTESIAN_POINT('Ctrl Pts',(15.5619966081066,-40.0501075176709,-1.06505331305163));
#6238=CARTESIAN_POINT('Ctrl Pts',(15.5498222393783,-40.088953757816,-1.0201422978767));
#6239=CARTESIAN_POINT('Ctrl Pts',(15.5393951597974,-40.1269007411589,-0.973968206823742));
#6240=CARTESIAN_POINT('Ctrl Pts',(15.528958825692,-40.1648814042379,-0.927753134088986));
#6241=CARTESIAN_POINT('Ctrl Pts',(15.520273092198,-40.201960656485,-0.880273333152562));
#6242=CARTESIAN_POINT('Ctrl Pts',(15.5133886580473,-40.2379301825509,-0.831792563199941));
#6243=CARTESIAN_POINT('Ctrl Pts',(15.5065094676442,-40.2738723112865,-0.78334872016332));
#6244=CARTESIAN_POINT('Ctrl Pts',(15.50142888499,-40.3087059338662,-0.733906126190651));
#6245=CARTESIAN_POINT('Ctrl Pts',(15.4981573254988,-40.3422489797573,-0.683748572306699));
#6246=CARTESIAN_POINT('Ctrl Pts',(15.494887629273,-40.375772921733,-0.633619584870454));
#6247=CARTESIAN_POINT('Ctrl Pts',(15.4934248002907,-40.4080074037208,-0.582777184218984));
#6248=CARTESIAN_POINT('Ctrl Pts',(15.4937394369914,-40.4388026103992,-0.531514551846304));
#6249=CARTESIAN_POINT('Ctrl Pts',(15.4938090605188,-40.4456170440328,-0.520171039531854));
#6250=CARTESIAN_POINT('Ctrl Pts',(15.4939655687831,-40.4523611372968,-0.50880696400498));
#6251=CARTESIAN_POINT('Ctrl Pts',(15.4942083905324,-40.4590335018639,-0.49742551165457));
#6252=CARTESIAN_POINT('Ctrl Pts',(15.4953058344853,-40.4891895573443,-0.445986519513396));
#6253=CARTESIAN_POINT('Ctrl Pts',(15.4984396882371,-40.5186182216488,-0.393696645408317));
#6254=CARTESIAN_POINT('Ctrl Pts',(15.5036405113949,-40.5471378008383,-0.340828125587056));
#6255=CARTESIAN_POINT('Ctrl Pts',(15.508843150823,-40.5756673398482,-0.287941142626714));
#6256=CARTESIAN_POINT('Ctrl Pts',(15.5161143164105,-40.6032866955214,-0.234475768275153));
#6257=CARTESIAN_POINT('Ctrl Pts',(15.5254390386774,-40.6298299707505,-0.180724039812537));
#6258=CARTESIAN_POINT('Ctrl Pts',(15.5347720370746,-40.6563968043871,-0.126924604158004));
#6259=CARTESIAN_POINT('Ctrl Pts',(15.5461621861609,-40.6818852404221,-0.0728390372964673));
#6260=CARTESIAN_POINT('Ctrl Pts',(15.5595483775206,-40.7061515153927,-0.018769220632637));
#6261=CARTESIAN_POINT('Ctrl Pts',(15.572924372863,-40.7303993071853,0.0352594120403899));
#6262=CARTESIAN_POINT('Ctrl Pts',(15.5882931376616,-40.7534264935081,0.0892715721474465));
#6263=CARTESIAN_POINT('Ctrl Pts',(15.6055498705326,-40.7751175242776,0.142968160451429));
#6264=CARTESIAN_POINT('Ctrl Pts',(15.6227967751024,-40.796796201261,0.196634166706726));
#6265=CARTESIAN_POINT('Ctrl Pts',(15.641929118661,-40.8171400548386,0.249984259989185));
#6266=CARTESIAN_POINT('Ctrl Pts',(15.6628030948396,-40.836065321335,0.302732839448093));
#6267=CARTESIAN_POINT('Ctrl Pts',(15.66742213594,-40.8402531475084,0.314405165526342));
#6268=CARTESIAN_POINT('Ctrl Pts',(15.6721263189559,-40.8443716395307,0.32604811133055));
#6269=CARTESIAN_POINT('Ctrl Pts',(15.676913858231,-40.8484201102111,0.337658719487509));
#6270=CARTESIAN_POINT('Ctrl Pts',(15.6985513599794,-40.8667173577936,0.39013339172803));
#6271=CARTESIAN_POINT('Ctrl Pts',(15.722362551344,-40.8842079556607,0.442451690705955));
#6272=CARTESIAN_POINT('Ctrl Pts',(15.748265636864,-40.9007750781021,0.494317440109603));
#6273=CARTESIAN_POINT('Ctrl Pts',(15.7741777684528,-40.9173479862377,0.546201302457251));
#6274=CARTESIAN_POINT('Ctrl Pts',(15.8021830926676,-40.9329964698455,0.59763156288463));
#6275=CARTESIAN_POINT('Ctrl Pts',(15.83215090363,-40.9476214522587,0.648314739712493));
#6276=CARTESIAN_POINT('Ctrl Pts',(15.8621453124374,-40.9622594150332,0.699042900249139));
#6277=CARTESIAN_POINT('Ctrl Pts',(15.894105351942,-40.9758718192981,0.749021923203392));
#6278=CARTESIAN_POINT('Ctrl Pts',(15.9278548543797,-40.9883813311363,0.797971596265911));
#6279=CARTESIAN_POINT('Ctrl Pts',(15.9615786504381,-41.000881314708,0.846883985257014));
#6280=CARTESIAN_POINT('Ctrl Pts',(15.9970886749691,-41.0122799393024,0.894767940773897));
#6281=CARTESIAN_POINT('Ctrl Pts',(16.0341705677136,-41.022524908682,0.941368295639198));
#6282=CARTESIAN_POINT('Ctrl Pts',(16.0712313410483,-41.0327640432001,0.98794211000402));
#6283=CARTESIAN_POINT('Ctrl Pts',(16.1098615702851,-41.0418507872325,1.03323325564664));
#6284=CARTESIAN_POINT('Ctrl Pts',(16.1498172223449,-41.0497592430222,1.07702027911083));
#6285=CARTESIAN_POINT('Ctrl Pts',(16.1586587002461,-41.0515092441733,1.08670957162287));
#6286=CARTESIAN_POINT('Ctrl Pts',(16.1675649833532,-41.0532016525781,1.09632535949797));
#6287=CARTESIAN_POINT('Ctrl Pts',(16.1765332779228,-41.0548363630651,1.10586550012264));
#6288=CARTESIAN_POINT('Ctrl Pts',(16.2170658935834,-41.0622245115445,1.14898260006709));
#6289=CARTESIAN_POINT('Ctrl Pts',(16.2595174031787,-41.0689531166638,1.1909670431649));
#6290=CARTESIAN_POINT('Ctrl Pts',(16.3036957872465,-41.0749689905696,1.23155737439127));
#6291=CARTESIAN_POINT('Ctrl Pts',(16.3478895996191,-41.0809869653838,1.27216188087589));
#6292=CARTESIAN_POINT('Ctrl Pts',(16.3938110523704,-41.0862915673586,1.31137063355205));
#6293=CARTESIAN_POINT('Ctrl Pts',(16.4412246219907,-41.0908442363149,1.3489468339874));
#6294=CARTESIAN_POINT('Ctrl Pts',(16.4886802733888,-41.0954009459794,1.38655638507171));
#6295=CARTESIAN_POINT('Ctrl Pts',(16.5376300920798,-41.0992042966577,1.42252990566999));
#6296=CARTESIAN_POINT('Ctrl Pts',(16.5878023876649,-41.1022321044514,1.45666435205266));
#6297=CARTESIAN_POINT('Ctrl Pts',(16.6379364679291,-41.1052576060193,1.49077279885112));
#6298=CARTESIAN_POINT('Ctrl Pts',(16.6892904409661,-41.1075087226786,1.52304454512959));
#6299=CARTESIAN_POINT('Ctrl Pts',(16.7415677450431,-41.1089806172348,1.55331889475933));
#6300=CARTESIAN_POINT('Ctrl Pts',(16.7938152754033,-41.1104516734967,1.58357600210906));
#6301=CARTESIAN_POINT('Ctrl Pts',(16.846984308073,-41.1111444354538,1.61183773325848));
#6302=CARTESIAN_POINT('Ctrl Pts',(16.9007646124888,-41.1110712244847,1.63799064371879));
#6303=CARTESIAN_POINT('Ctrl Pts',(16.9126652410207,-41.1110550241943,1.64377781944784));
#6304=CARTESIAN_POINT('Ctrl Pts',(16.9245957720954,-41.1110013822196,1.64946192467195));
#6305=CARTESIAN_POINT('Ctrl Pts',(16.9365528098639,-41.1109105410149,1.65504205590818));
#6306=CARTESIAN_POINT('Ctrl Pts',(16.9905931865084,-41.1104999800539,1.68026171311506));
#6307=CARTESIAN_POINT('Ctrl Pts',(17.0459560513166,-41.1097742107652,1.70359676647086));
#6308=CARTESIAN_POINT('Ctrl Pts',(17.1023631231069,-41.1087298485223,1.72487226661194));
#6309=CARTESIAN_POINT('Ctrl Pts',(17.1587898937959,-41.1076851215595,1.746155196742));
#6310=CARTESIAN_POINT('Ctrl Pts',(17.2162609360078,-41.1063215649501,1.76537666733503));
#6311=CARTESIAN_POINT('Ctrl Pts',(17.2744675877866,-41.1046428450168,1.78240346403918));
#6312=CARTESIAN_POINT('Ctrl Pts',(17.332725900712,-41.1029626351404,1.79944537282785));
#6313=CARTESIAN_POINT('Ctrl Pts',(17.3917203532226,-41.1009667137788,1.81428839412925));
#6314=CARTESIAN_POINT('Ctrl Pts',(17.4511221884286,-41.0986658443878,1.82684686809438));
#6315=CARTESIAN_POINT('Ctrl Pts',(17.5104787783426,-41.096366727527,1.83939577649946));
#6316=CARTESIAN_POINT('Ctrl Pts',(17.5702413003446,-41.0937631661781,1.84966349840239));
#6317=CARTESIAN_POINT('Ctrl Pts',(17.6300746296397,-41.0908725875409,1.85761563656216));
#6318=CARTESIAN_POINT('Ctrl Pts',(17.6898738818011,-41.0879836551874,1.86556324570646));
#6319=CARTESIAN_POINT('Ctrl Pts',(17.7497430473289,-41.0848080936348,1.87119797990062));
#6320=CARTESIAN_POINT('Ctrl Pts',(17.8093528386257,-41.0813692268452,1.87453687269556));
#6321=CARTESIAN_POINT('Ctrl Pts',(17.8225434293238,-41.0806082665516,1.87527571051541));
#6322=CARTESIAN_POINT('Ctrl Pts',(17.8357213668488,-41.0798344341278,1.87590232633982));
#6323=CARTESIAN_POINT('Ctrl Pts',(17.8488831784817,-41.0790480164089,1.87641723476232));
#6324=CARTESIAN_POINT('Ctrl Pts',(17.9083685854582,-41.0754937657201,1.87874438682333));
#6325=CARTESIAN_POINT('Ctrl Pts',(17.9683565902155,-41.0720976706368,1.87880825693467));
#6326=CARTESIAN_POINT('Ctrl Pts',(18.028523697326,-41.0688824509898,1.87655505226089));
#6327=CARTESIAN_POINT('Ctrl Pts',(18.0887118164424,-41.0656661084998,1.87430106070616));
#6328=CARTESIAN_POINT('Ctrl Pts',(18.1490783712004,-41.0626308269423,1.86972820122929));
#6329=CARTESIAN_POINT('Ctrl Pts',(18.2092877263486,-41.0597958456794,1.86283322829508));
#6330=CARTESIAN_POINT('Ctrl Pts',(18.2695505201376,-41.056958348237,1.85593213574738));
#6331=CARTESIAN_POINT('Ctrl Pts',(18.3296549981847,-41.0543215533332,1.84670481534557));
#6332=CARTESIAN_POINT('Ctrl Pts',(18.3892650959712,-41.0519004434854,1.83519995710487));
#6333=CARTESIAN_POINT('Ctrl Pts',(18.4488297898368,-41.0494811777526,1.82370386190423));
#6334=CARTESIAN_POINT('Ctrl Pts',(18.5079000450163,-41.0472772968405,1.80993391118287));
#6335=CARTESIAN_POINT('Ctrl Pts',(18.566153449952,-41.045298887958,1.793988819383));
#6336=CARTESIAN_POINT('Ctrl Pts',(18.6243736775742,-41.0433216058472,1.77805280886017));
#6337=CARTESIAN_POINT('Ctrl Pts',(18.6817772619035,-41.0415695482632,1.75994451788674));
#6338=CARTESIAN_POINT('Ctrl Pts',(18.7380667732378,-41.0400476460038,1.73980808434969));
#6339=CARTESIAN_POINT('Ctrl Pts',(18.7505226448052,-41.0397108759976,1.73535224836857));
#6340=CARTESIAN_POINT('Ctrl Pts',(18.7629240831117,-41.039385355606,1.73079726584407));
#6341=CARTESIAN_POINT('Ctrl Pts',(18.7752680790298,-41.0390711040097,1.72614496752461));
#6342=CARTESIAN_POINT('Ctrl Pts',(18.8310573306497,-41.0376508296109,1.70511869343333));
#6343=CARTESIAN_POINT('Ctrl Pts',(18.8864681944013,-41.0368973481195,1.68189873004126));
#6344=CARTESIAN_POINT('Ctrl Pts',(18.94118196332,-41.0368306147455,1.65656309537192));
#6345=CARTESIAN_POINT('Ctrl Pts',(18.9959148397898,-41.0367638580664,1.63121861280294));
#6346=CARTESIAN_POINT('Ctrl Pts',(19.0499493384097,-41.0373843908253,1.60375713415765));
#6347=CARTESIAN_POINT('Ctrl Pts',(19.1029743581755,-41.0386972875298,1.57430602553558));
#6348=CARTESIAN_POINT('Ctrl Pts',(19.1560464401448,-41.040011349492,1.54482877766693));
#6349=CARTESIAN_POINT('Ctrl Pts',(19.2081064812735,-41.0420190124084,1.51335869953315));
#6350=CARTESIAN_POINT('Ctrl Pts',(19.2588623156411,-41.0447099139289,1.48006918735906));
#6351=CARTESIAN_POINT('Ctrl Pts',(19.3095794902174,-41.0473987658389,1.44680503119789));
#6352=CARTESIAN_POINT('Ctrl Pts',(19.3589937747191,-41.0507697621964,1.41172471547047));
#6353=CARTESIAN_POINT('Ctrl Pts',(19.4068442291116,-41.0547974996097,1.37504051469626));
#6354=CARTESIAN_POINT('Ctrl Pts',(19.4546674310289,-41.0588229430885,1.33837720683284));
#6355=CARTESIAN_POINT('Ctrl Pts',(19.5009280586969,-41.0635042745324,1.30011245980285));
#6356=CARTESIAN_POINT('Ctrl Pts',(19.5454051453916,-41.0688022788184,1.26048896755312));
#6357=CARTESIAN_POINT('Ctrl Pts',(19.5552471366694,-41.0699746333013,1.25172099073414));
#6358=CARTESIAN_POINT('Ctrl Pts',(19.5650019652858,-41.0711771337269,1.24288658001268));
#6359=CARTESIAN_POINT('Ctrl Pts',(19.5746675343455,-41.0724092725985,1.2339885196899));
#6360=CARTESIAN_POINT('Ctrl Pts',(19.6183515138191,-41.0779779803321,1.1937733309004));
#6361=CARTESIAN_POINT('Ctrl Pts',(19.6608895145212,-41.0846566497875,1.15186853252883));
#6362=CARTESIAN_POINT('Ctrl Pts',(19.702016672246,-41.0924341500438,1.10846850103133));
#6363=CARTESIAN_POINT('Ctrl Pts',(19.7431581927032,-41.1002143664166,1.06505331305146));
#6364=CARTESIAN_POINT('Ctrl Pts',(19.7828872078737,-41.1090941738953,1.0201422978774));
#6365=CARTESIAN_POINT('Ctrl Pts',(19.8209637992355,-41.1190375497622,0.973968206825355));
#6366=CARTESIAN_POINT('Ctrl Pts',(19.8590741853671,-41.1289897508439,0.927753134090774));
#6367=CARTESIAN_POINT('Ctrl Pts',(19.8955286265134,-41.1400073111111,0.880273333154538));
#6368=CARTESIAN_POINT('Ctrl Pts',(19.9301213669238,-41.1520299792788,0.831792563202099));
#6369=CARTESIAN_POINT('Ctrl Pts',(19.964687758676,-41.1640434899999,0.783348720166139));
#6370=CARTESIAN_POINT('Ctrl Pts',(19.9973948520627,-41.177060387645,0.73390612619414));
#6371=CARTESIAN_POINT('Ctrl Pts',(20.02807976167,-41.1909986569609,0.683748572310881));
#6372=CARTESIAN_POINT('Ctrl Pts',(20.0587471951687,-41.2049289879544,0.63361958487495));
#6373=CARTESIAN_POINT('Ctrl Pts',(20.0873944899392,-41.2197793818882,0.582777184223805));
#6374=CARTESIAN_POINT('Ctrl Pts',(20.1139066028871,-41.235449468603,0.531514551851436));
#6375=CARTESIAN_POINT('Ctrl Pts',(20.1197732637633,-41.2389169811637,0.520171039535283));
#6376=CARTESIAN_POINT('Ctrl Pts',(20.1255355657243,-41.242424567929,0.508806964006691));
#6377=CARTESIAN_POINT('Ctrl Pts',(20.1311925920688,-41.2459710400166,0.497425511654565));
#6378=CARTESIAN_POINT('Ctrl Pts',(20.1567597802162,-41.2619994820991,0.445986519513783));
#6379=CARTESIAN_POINT('Ctrl Pts',(20.1806788242272,-41.279427811212,0.393696645409107));
#6380=CARTESIAN_POINT('Ctrl Pts',(20.2027770927316,-41.2981916457819,0.340828125588261));
#6381=CARTESIAN_POINT('Ctrl Pts',(20.2248830785584,-41.3169620331983,0.287941142627905));
#6382=CARTESIAN_POINT('Ctrl Pts',(20.2451665594138,-41.3370687251488,0.234475768276321));
#6383=CARTESIAN_POINT('Ctrl Pts',(20.2634913489284,-41.3584158091296,0.180724039813684));
#6384=CARTESIAN_POINT('Ctrl Pts',(20.2818324025573,-41.3797818396534,0.126924604159152));
#6385=CARTESIAN_POINT('Ctrl Pts',(20.2982109611232,-41.4023902161325,0.0728390372976226));
#6386=CARTESIAN_POINT('Ctrl Pts',(20.3125330760231,-41.4261161353952,0.0187692206337898));
#6387=CARTESIAN_POINT('Ctrl Pts',(20.3268442820301,-41.4498239830589,-0.0352594120392662));
#6388=CARTESIAN_POINT('Ctrl Pts',(20.339102027964,-41.4746473169607,-0.0892715721463639));
#6389=CARTESIAN_POINT('Ctrl Pts',(20.3492586452092,-41.5004376013981,-0.142968160450382));
#6390=CARTESIAN_POINT('Ctrl Pts',(20.3594094779124,-41.5262131973838,-0.196634166705389));
#6391=CARTESIAN_POINT('Ctrl Pts',(20.3674616001421,-41.552954219728,-0.24998425998755));
#6392=CARTESIAN_POINT('Ctrl Pts',(20.3734143736121,-41.5804942466247,-0.302732839446182));
#6393=CARTESIAN_POINT('Ctrl Pts',(20.3747316169147,-41.5865883666458,-0.314405165525066));
#6394=CARTESIAN_POINT('Ctrl Pts',(20.3759462441234,-41.5927215546531,-0.326048111329918));
#6395=CARTESIAN_POINT('Ctrl Pts',(20.3770585529417,-41.5988919206274,-0.337658719487506));
#6396=CARTESIAN_POINT('Ctrl Pts',(20.3820856832934,-41.6267791706076,-0.39013339172863));
#6397=CARTESIAN_POINT('Ctrl Pts',(20.3853273896913,-41.6561455661577,-0.442451690707166));
#6398=CARTESIAN_POINT('Ctrl Pts',(20.3867233958332,-41.6868618574755,-0.494317440111406));
#6399=CARTESIAN_POINT('Ctrl Pts',(20.3881198894988,-41.7175888757661,-0.546201302460337));
#6400=CARTESIAN_POINT('Ctrl Pts',(20.3876692117263,-41.7496664397822,-0.597631562888963));
#6401=CARTESIAN_POINT('Ctrl Pts',(20.3853509125446,-41.7829318165789,-0.648314739718037));
#6402=CARTESIAN_POINT('Ctrl Pts',(20.3830305557632,-41.816226717965,-0.699042900254785));
#6403=CARTESIAN_POINT('Ctrl Pts',(20.3788392239107,-41.8507111262147,-0.749021923209121));
#6404=CARTESIAN_POINT('Ctrl Pts',(20.3727980277325,-41.8861938086101,-0.797971596271709));
#6405=CARTESIAN_POINT('Ctrl Pts',(20.3667614330232,-41.9216494644944,-0.846883985262495));
#6406=CARTESIAN_POINT('Ctrl Pts',(20.3588779192245,-41.9581013601243,-0.894767940779068));
#6407=CARTESIAN_POINT('Ctrl Pts',(20.3492093765959,-41.9953377059512,-0.941368295644055));
#6408=CARTESIAN_POINT('Ctrl Pts',(20.3395463405339,-42.0325528444024,-0.987942110009238));
#6409=CARTESIAN_POINT('Ctrl Pts',(20.3281005770849,-42.0705509762921,-1.03323325565219));
#6410=CARTESIAN_POINT('Ctrl Pts',(20.3149716746733,-42.1091078138959,-1.07702027911667));
#6411=CARTESIAN_POINT('Ctrl Pts',(20.3120664811768,-42.1176397589392,-1.08670957162673));
#6412=CARTESIAN_POINT('Ctrl Pts',(20.3090790082959,-42.1261990305639,-1.09632535949989));
#6413=CARTESIAN_POINT('Ctrl Pts',(20.3060105618213,-42.1347831567316,-1.10586550012264));
#6414=CARTESIAN_POINT('Ctrl Pts',(20.2921425782615,-42.1735795058142,-1.148982600066));
#6415=CARTESIAN_POINT('Ctrl Pts',(20.2767439664296,-42.2137078941114,-1.19096704316276));
#6416=CARTESIAN_POINT('Ctrl Pts',(20.2598646740246,-42.254975433964,-1.23155737438818));
#6417=CARTESIAN_POINT('Ctrl Pts',(20.2429794869067,-42.296257385576,-1.27216188087308));
#6418=CARTESIAN_POINT('Ctrl Pts',(20.2246126805982,-42.3386788312249,-1.31137063354952));
#6419=CARTESIAN_POINT('Ctrl Pts',(20.2048486227591,-42.3820165214785,-1.34894683398513));
#6420=CARTESIAN_POINT('Ctrl Pts',(20.1850670233874,-42.4253926759745,-1.38655638506932));
#6421=CARTESIAN_POINT('Ctrl Pts',(20.1638859123489,-42.4696861378104,-1.42252990566751));
#6422=CARTESIAN_POINT('Ctrl Pts',(20.1414219230237,-42.5146505242499,-1.45666435205011));
#6423=CARTESIAN_POINT('Ctrl Pts',(20.1189750441085,-42.5595806621383,-1.49077279884886));
#6424=CARTESIAN_POINT('Ctrl Pts',(20.0952475818038,-42.6051800657034,-1.5230445451276));
#6425=CARTESIAN_POINT('Ctrl Pts',(20.0703836278425,-42.6511894863539,-1.5533188947576));
#6426=CARTESIAN_POINT('Ctrl Pts',(20.0455338347557,-42.6971727030616,-1.58357600210732));
#6427=CARTESIAN_POINT('Ctrl Pts',(20.0195492678746,-42.7435648170265,-1.61183773325675));
#6428=CARTESIAN_POINT('Ctrl Pts',(19.9925957131078,-42.7901033213892,-1.63799064371707));
#6429=CARTESIAN_POINT('Ctrl Pts',(19.9866313689782,-42.8004014678746,-1.64377781944672));
#6430=CARTESIAN_POINT('Ctrl Pts',(19.9806196481275,-42.8107067898797,-1.6494619246714));
#6431=CARTESIAN_POINT('Ctrl Pts',(19.9745624584516,-42.8210164677399,-1.65504205590818));
#6432=CARTESIAN_POINT('Ctrl Pts',(19.9471867139073,-42.8676115262635,-1.68026171311505));
#6433=CARTESIAN_POINT('Ctrl Pts',(19.9188767468619,-42.9151942889694,-1.70359676647086));
#6434=CARTESIAN_POINT('Ctrl Pts',(19.8897687667337,-42.9635220649715,-1.72487226661194));
#6435=CARTESIAN_POINT('Ctrl Pts',(19.8606506212993,-43.0118667183605,-1.7461551967421));
#6436=CARTESIAN_POINT('Ctrl Pts',(19.8307342255299,-43.0609563225936,-1.76537666733522));
#6437=CARTESIAN_POINT('Ctrl Pts',(19.8001770855323,-43.1105254017368,-1.78240346403943));
#6438=CARTESIAN_POINT('Ctrl Pts',(19.7695928246328,-43.1601384757738,-1.79944537282815));
#6439=CARTESIAN_POINT('Ctrl Pts',(19.7383670797743,-43.2102312096498,-1.81428839412959));
#6440=CARTESIAN_POINT('Ctrl Pts',(19.7066735508277,-43.2605242732743,-1.82684686809472));
#6441=CARTESIAN_POINT('Ctrl Pts',(19.6750041622631,-43.3107790295912,-1.83939577649969));
#6442=CARTESIAN_POINT('Ctrl Pts',(19.6428681509939,-43.3612331111643,-1.84966349840252));
#6443=CARTESIAN_POINT('Ctrl Pts',(19.6104481718151,-43.4116050050079,-1.85761563656223));
#6444=CARTESIAN_POINT('Ctrl Pts',(19.5780466569263,-43.4619482103305,-1.86556324570655));
#6445=CARTESIAN_POINT('Ctrl Pts',(19.5453619571864,-43.5122086478048,-1.87119797990071));
#6446=CARTESIAN_POINT('Ctrl Pts',(19.5125789155379,-43.5621128079876,-1.87453687269564));
#6447=CARTESIAN_POINT('Ctrl Pts',(19.5053246092435,-43.573155714476,-1.87527571051545));
#6448=CARTESIAN_POINT('Ctrl Pts',(19.498065481944,-43.5841812269298,-1.87590232633983));
#6449=CARTESIAN_POINT('Ctrl Pts',(19.4908035184053,-43.5951864813039,-1.87641723476232));
#6450=CARTESIAN_POINT('Ctrl Pts',(19.4579827435292,-43.6449252295553,-1.87874438682332));
#6451=CARTESIAN_POINT('Ctrl Pts',(19.4250476365349,-43.6951783180556,-1.87880825693467));
#6452=CARTESIAN_POINT('Ctrl Pts',(19.3921796210868,-43.7456769514617,-1.87655505226092));
#6453=CARTESIAN_POINT('Ctrl Pts',(19.3593001272252,-43.7961932203771,-1.87430106070623));
#6454=CARTESIAN_POINT('Ctrl Pts',(19.3264882189101,-43.8469545495574,-1.86972820122944));
#6455=CARTESIAN_POINT('Ctrl Pts',(19.2939283755433,-43.8976798900294,-1.86283322829534));
#6456=CARTESIAN_POINT('Ctrl Pts',(19.2613396337806,-43.9484502516322,-1.85593213574773));
#6457=CARTESIAN_POINT('Ctrl Pts',(19.2290038633859,-43.9991838590501,-1.84670481534603));
#6458=CARTESIAN_POINT('Ctrl Pts',(19.1971020718592,-44.0495971631312,-1.83519995710545));
#6459=CARTESIAN_POINT('Ctrl Pts',(19.165224579344,-44.0999720683201,-1.8237038619051));
#6460=CARTESIAN_POINT('Ctrl Pts',(19.1337808348979,-44.1500264694566,-1.80993391118412));
#6461=CARTESIAN_POINT('Ctrl Pts',(19.1029407800793,-44.1994861935458,-1.79398881938471));
#6462=CARTESIAN_POINT('Ctrl Pts',(19.0721182897293,-44.2489177486262,-1.77805280886179));
#6463=CARTESIAN_POINT('Ctrl Pts',(19.0418991711875,-44.2977546821324,-1.7599445178882));
#6464=CARTESIAN_POINT('Ctrl Pts',(19.0124364095012,-44.3457418777856,-1.73980808435093));
#6465=CARTESIAN_POINT('Ctrl Pts',(19.0059168223362,-44.3563605939871,-1.73535224836942));
#6466=CARTESIAN_POINT('Ctrl Pts',(18.9994341942538,-44.3669377944092,-1.7307972658445));
#6467=CARTESIAN_POINT('Ctrl Pts',(18.9929900464286,-44.3774708826612,-1.72614496752462));
#6468=CARTESIAN_POINT('Ctrl Pts',(18.9638689474167,-44.4250699002826,-1.70512123503431));
#6469=CARTESIAN_POINT('Ctrl Pts',(18.9355143751871,-44.4726744936063,-1.6819044064235));
#6470=CARTESIAN_POINT('Ctrl Pts',(18.9081029063368,-44.5200187400556,-1.65657248784969));
#6471=CARTESIAN_POINT('Ctrl Pts',(18.8806675607685,-44.5674042256384,-1.63121850394697));
#6472=CARTESIAN_POINT('Ctrl Pts',(18.8541774156252,-44.6145282512141,-1.60374589296114));
#6473=CARTESIAN_POINT('Ctrl Pts',(18.8287926096657,-44.6611236299078,-1.57428219817154));
#6474=CARTESIAN_POINT('Ctrl Pts',(18.8184986722539,-44.6800187876141,-1.56233420729198));
#6475=CARTESIAN_POINT('Ctrl Pts',(18.8083862688025,-44.6988270623412,-1.55005934730935));
#6476=CARTESIAN_POINT('Ctrl Pts',(18.7984650370909,-44.7175309941718,-1.53746830583367));
#6477=CARTESIAN_POINT('Origin',(18.8566790438274,-45.0585105479845,-1.8991695164178));
#6478=CARTESIAN_POINT('Ctrl Pts',(3.23546955922299,-20.8337067011995,-0.275782109461828));
#6479=CARTESIAN_POINT('Ctrl Pts',(3.24186862921633,-20.8593806772798,-0.20661167837916));
#6480=CARTESIAN_POINT('Ctrl Pts',(3.25061275091574,-20.8836022411874,-0.13722900415027));
#6481=CARTESIAN_POINT('Ctrl Pts',(3.26163446655099,-20.9062743501088,-0.0679614783569666));
#6482=CARTESIAN_POINT('Ctrl Pts',(3.27267218983593,-20.9289793874045,0.00140664976769637));
#6483=CARTESIAN_POINT('Ctrl Pts',(3.2859938790503,-20.9501303415672,0.0706586286035451));
#6484=CARTESIAN_POINT('Ctrl Pts',(3.30149075533669,-20.9696606976443,0.139474749410477));
#6485=CARTESIAN_POINT('Ctrl Pts',(3.30349716107535,-20.9721893245615,0.148384484323984));
#6486=CARTESIAN_POINT('Ctrl Pts',(3.30553997633814,-20.9746908292539,0.157286933483624));
#6487=CARTESIAN_POINT('Ctrl Pts',(3.30761891872921,-20.9771651064803,0.166181422977341));
#6488=CARTESIAN_POINT('Ctrl Pts',(3.32367525640493,-20.9962747416586,0.234876412977235));
#6489=CARTESIAN_POINT('Ctrl Pts',(3.34225287296391,-21.0143094751689,0.303705335324898));
#6490=CARTESIAN_POINT('Ctrl Pts',(3.36331943904694,-21.0311598985507,0.372344470076959));
#6491=CARTESIAN_POINT('Ctrl Pts',(3.38435814667915,-21.0479880389137,0.440892836359587));
#6492=CARTESIAN_POINT('Ctrl Pts',(3.40787918918959,-21.0636347575442,0.509251242356875));
#6493=CARTESIAN_POINT('Ctrl Pts',(3.43380253213101,-21.078010950724,0.577093346534907));
#6494=CARTESIAN_POINT('Ctrl Pts',(3.45972752251918,-21.0923880575211,0.644939762126552));
#6495=CARTESIAN_POINT('Ctrl Pts',(3.48805494275311,-21.1054942936163,0.712269124557974));
#6496=CARTESIAN_POINT('Ctrl Pts',(3.51865844890996,-21.1172636372539,0.778761359262223));
#6497=CARTESIAN_POINT('Ctrl Pts',(3.54925455115654,-21.1290301335326,0.845237507491391));
#6498=CARTESIAN_POINT('Ctrl Pts',(3.58212531838659,-21.1394602771986,0.910876280137527));
#6499=CARTESIAN_POINT('Ctrl Pts',(3.61710196385512,-21.1485133692941,0.975374241033912));
#6500=CARTESIAN_POINT('Ctrl Pts',(3.65213177087612,-21.1575802213264,1.03997023339348));
#6501=CARTESIAN_POINT('Ctrl Pts',(3.68927343113846,-21.1652658000617,1.10342135481118));
#6502=CARTESIAN_POINT('Ctrl Pts',(3.7283203630776,-21.1715556385076,1.16544861040201));
#6503=CARTESIAN_POINT('Ctrl Pts',(3.75451366980928,-21.1757749627804,1.20705748594561));
#6504=CARTESIAN_POINT('Ctrl Pts',(3.78156357052937,-21.179366767248,1.24802618569455));
#6505=CARTESIAN_POINT('Ctrl Pts',(3.80940000840298,-21.1823333185883,1.28827884419633));
#6506=CARTESIAN_POINT('Ctrl Pts',(3.85089568313003,-21.186755545672,1.3482833329773));
#6507=CARTESIAN_POINT('Ctrl Pts',(3.89472960492292,-21.1902085445568,1.4072279179729));
#6508=CARTESIAN_POINT('Ctrl Pts',(3.94074551483351,-21.1926544575637,1.46480935021334));
#6509=CARTESIAN_POINT('Ctrl Pts',(3.98670057325282,-21.1950971360925,1.52231463670269));
#6510=CARTESIAN_POINT('Ctrl Pts',(4.03483155540641,-21.1965352994454,1.57845972694472));
#6511=CARTESIAN_POINT('Ctrl Pts',(4.08493792610339,-21.1969494150408,1.63296134034075));
#6512=CARTESIAN_POINT('Ctrl Pts',(4.13504748109556,-21.1973635569535,1.68746641735274));
#6513=CARTESIAN_POINT('Ctrl Pts',(4.18713224730921,-21.1967534829521,1.74032721705632));
#6514=CARTESIAN_POINT('Ctrl Pts',(4.24095216427237,-21.195118825561,1.79128851362552));
#6515=CARTESIAN_POINT('Ctrl Pts',(4.29475906057596,-21.1934845636428,1.84223748112157));
#6516=CARTESIAN_POINT('Ctrl Pts',(4.35029972224413,-21.1908262376525,1.89128737321195));
#6517=CARTESIAN_POINT('Ctrl Pts',(4.40730213618998,-21.1871627463886,1.9382193964011));
#6518=CARTESIAN_POINT('Ctrl Pts',(4.46439118899948,-21.1834936869267,1.98522275230891));
#6519=CARTESIAN_POINT('Ctrl Pts',(4.52294581901202,-21.1788164818126,2.03010142110727));
#6520=CARTESIAN_POINT('Ctrl Pts',(4.58266933425896,-21.1731686893198,2.07267852251363));
#6521=CARTESIAN_POINT('Ctrl Pts',(4.62273282391777,-21.1693800597458,2.10123992340978));
#6522=CARTESIAN_POINT('Ctrl Pts',(4.66332182748729,-21.1651550595386,2.12876654161616));
#6523=CARTESIAN_POINT('Ctrl Pts',(4.70434308191444,-21.1605093534924,2.15521684061908));
#6524=CARTESIAN_POINT('Ctrl Pts',(4.76549331379183,-21.1535840167146,2.19464620327124));
#6525=CARTESIAN_POINT('Ctrl Pts',(4.82836829765705,-21.1460436532863,2.23203175294848));
#6526=CARTESIAN_POINT('Ctrl Pts',(4.89270780991765,-21.1379104295439,2.26715077383212));
#6527=CARTESIAN_POINT('Ctrl Pts',(4.95696223953439,-21.1297879611859,2.30222335328279));
#6528=CARTESIAN_POINT('Ctrl Pts',(5.02267680474199,-21.1210742381291,2.33503490407264));
#6529=CARTESIAN_POINT('Ctrl Pts',(5.08955858326424,-21.1118030675008,2.36540131373504));
#6530=CARTESIAN_POINT('Ctrl Pts',(5.15644461217079,-21.102531307683,2.39576965320423));
#6531=CARTESIAN_POINT('Ctrl Pts',(5.2244973822523,-21.0927021023501,2.42369216050349));
#6532=CARTESIAN_POINT('Ctrl Pts',(5.29339874516216,-21.0823601680819,2.44902900915281));
#6533=CARTESIAN_POINT('Ctrl Pts',(5.36228343875623,-21.0720207358393,2.47435972805499));
#6534=CARTESIAN_POINT('Ctrl Pts',(5.43201562568106,-21.0611689289218,2.49710580690362));
#6535=CARTESIAN_POINT('Ctrl Pts',(5.50226209398045,-21.0498589793117,2.51717642960937));
#6536=CARTESIAN_POINT('Ctrl Pts',(5.57261533098965,-21.0385318395316,2.53727755796962));
#6537=CARTESIAN_POINT('Ctrl Pts',(5.6434837004336,-21.026745293642,2.55469500339243));
#6538=CARTESIAN_POINT('Ctrl Pts',(5.71452769367997,-21.0145616201289,2.56938903350696));
#6539=CARTESIAN_POINT('Ctrl Pts',(5.76218514111884,-21.0063886169864,2.57924602402578));
#6540=CARTESIAN_POINT('Ctrl Pts',(5.80992153437209,-20.9980370694213,2.5878785763622));
#6541=CARTESIAN_POINT('Ctrl Pts',(5.85763560155421,-20.9895272661294,2.59528770975726));
#6542=CARTESIAN_POINT('Ctrl Pts',(5.92876278458999,-20.9768417339146,2.60633247743794));
#6543=CARTESIAN_POINT('Ctrl Pts',(6.00069227149917,-20.9640737507165,2.61475432517954));
#6544=CARTESIAN_POINT('Ctrl Pts',(6.07310043046255,-20.9512820916283,2.62045518191383));
#6545=CARTESIAN_POINT('Ctrl Pts',(6.14541283679449,-20.9385073482445,2.62614849982872));
#6546=CARTESIAN_POINT('Ctrl Pts',(6.21820198419475,-20.9257091132545,2.6291277811253));
#6547=CARTESIAN_POINT('Ctrl Pts',(6.29112897535549,-20.912947737482,2.62934454720093));
#6548=CARTESIAN_POINT('Ctrl Pts',(6.36406060107808,-20.900185550715,2.6295613270522));
#6549=CARTESIAN_POINT('Ctrl Pts',(6.43712937391484,-20.8874603548411,2.62701514692945));
#6550=CARTESIAN_POINT('Ctrl Pts',(6.50999015258026,-20.8748324508206,2.62170927404782));
#6551=CARTESIAN_POINT('Ctrl Pts',(6.58283330402795,-20.8622076018706,2.61640468481672));
#6552=CARTESIAN_POINT('Ctrl Pts',(6.65546784140341,-20.8496801221392,2.60834181054528));
#6553=CARTESIAN_POINT('Ctrl Pts',(6.72755350254027,-20.8373083140492,2.59757579979075));
#6554=CARTESIAN_POINT('Ctrl Pts',(6.79974872780499,-20.824917701854,2.58679342560749));
#6555=CARTESIAN_POINT('Ctrl Pts',(6.87139271924896,-20.8126833503939,2.57329990897777));
#6556=CARTESIAN_POINT('Ctrl Pts',(6.94215892568192,-20.8006600571723,2.5572005349258));
#6557=CARTESIAN_POINT('Ctrl Pts',(6.9896300292816,-20.7925946396956,2.54640081720694));
#6558=CARTESIAN_POINT('Ctrl Pts',(7.03670647086889,-20.7846241154025,2.53442952081183));
#6559=CARTESIAN_POINT('Ctrl Pts',(7.08329575335921,-20.7767637068552,2.52133001886304));
#6560=CARTESIAN_POINT('Ctrl Pts',(7.15274622402516,-20.7650462249784,2.50180263987794));
#6561=CARTESIAN_POINT('Ctrl Pts',(7.22195029957584,-20.7538517587617,2.47959273545153));
#6562=CARTESIAN_POINT('Ctrl Pts',(7.29057405515975,-20.7432450259833,2.45474630344388));
#6563=CARTESIAN_POINT('Ctrl Pts',(7.3591070626117,-20.7326523195604,2.42993272838601));
#6564=CARTESIAN_POINT('Ctrl Pts',(7.42706058357602,-20.7226459347948,2.40248965699003));
#6565=CARTESIAN_POINT('Ctrl Pts',(7.49410526368581,-20.713280712891,2.37251384629915));
#6566=CARTESIAN_POINT('Ctrl Pts',(7.56115420453236,-20.7039148958208,2.34253613062434));
#6567=CARTESIAN_POINT('Ctrl Pts',(7.62729349814889,-20.69519043664,2.31002556527974));
#6568=CARTESIAN_POINT('Ctrl Pts',(7.69220745152933,-20.687150634337,2.27512786406365));
#6569=CARTESIAN_POINT('Ctrl Pts',(7.75710570026851,-20.6791127771045,2.240238605653));
#6570=CARTESIAN_POINT('Ctrl Pts',(7.82077856718671,-20.6717593202239,2.20296372939565));
#6571=CARTESIAN_POINT('Ctrl Pts',(7.88293428494723,-20.6651205676153,2.16349342564724));
#6572=CARTESIAN_POINT('Ctrl Pts',(7.94518447415883,-20.6584717246624,2.1239631303646));
#6573=CARTESIAN_POINT('Ctrl Pts',(8.00591234872199,-20.652539796222,2.08223120813799));
#6574=CARTESIAN_POINT('Ctrl Pts',(8.064857522614,-20.6473413793201,2.03852710839638));
#6575=CARTESIAN_POINT('Ctrl Pts',(8.10439888843787,-20.6438541980828,2.00920969898384));
#6576=CARTESIAN_POINT('Ctrl Pts',(8.14313874853075,-20.6406968013597,1.97900561592648));
#6577=CARTESIAN_POINT('Ctrl Pts',(8.18100842628527,-20.6378706589539,1.94799199564959));
#6578=CARTESIAN_POINT('Ctrl Pts',(8.23746061450179,-20.6336577389483,1.90176010689425));
#6579=CARTESIAN_POINT('Ctrl Pts',(8.29269916543629,-20.6305262721282,1.85331739425806));
#6580=CARTESIAN_POINT('Ctrl Pts',(8.34643501506069,-20.6285150758632,1.80284481408902));
#6581=CARTESIAN_POINT('Ctrl Pts',(8.40009980433667,-20.6265065392064,1.75243897891719));
#6582=CARTESIAN_POINT('Ctrl Pts',(8.45226524535692,-20.6256154066465,1.7000089916859));
#6583=CARTESIAN_POINT('Ctrl Pts',(8.50266515457153,-20.6258600476996,1.64577768116514));
#6584=CARTESIAN_POINT('Ctrl Pts',(8.55306826673607,-20.6261047042999,1.59154292420618));
#6585=CARTESIAN_POINT('Ctrl Pts',(8.60170506750094,-20.6274853140785,1.53550708982212));
#6586=CARTESIAN_POINT('Ctrl Pts',(8.64833992076498,-20.6299989551482,1.47792947798962));
#6587=CARTESIAN_POINT('Ctrl Pts',(8.69496349165288,-20.6325119880925,1.42036579591624));
#6588=CARTESIAN_POINT('Ctrl Pts',(8.73958563594783,-20.6361574710468,1.361261664062));
#6589=CARTESIAN_POINT('Ctrl Pts',(8.78200902118676,-20.6409111859313,1.30090464504851));
#6590=CARTESIAN_POINT('Ctrl Pts',(8.82449688639477,-20.6456721260617,1.24045588845447));
#6591=CARTESIAN_POINT('Ctrl Pts',(8.8647789760219,-20.6515445770579,1.17875107963639));
#6592=CARTESIAN_POINT('Ctrl Pts',(8.90270117211557,-20.658483782047,1.11609838715458));
#6593=CARTESIAN_POINT('Ctrl Pts',(8.92813998804528,-20.6631387117873,1.07406995853698));
#6594=CARTESIAN_POINT('Ctrl Pts',(8.95251779902157,-20.6682732479878,1.03161537789573));
#6595=CARTESIAN_POINT('Ctrl Pts',(8.97580007665302,-20.6738691449698,0.988830267143716));
#6596=CARTESIAN_POINT('Ctrl Pts',(9.01050688159292,-20.6822109278527,0.925050661183007));
#6597=CARTESIAN_POINT('Ctrl Pts',(9.04330583807951,-20.6920349669275,0.859969813685453));
#6598=CARTESIAN_POINT('Ctrl Pts',(9.07399901152766,-20.7033274659558,0.793867798863035));
#6599=CARTESIAN_POINT('Ctrl Pts',(9.10465159628846,-20.7146050317706,0.727853197419915));
#6600=CARTESIAN_POINT('Ctrl Pts',(9.13320352671783,-20.7273471659068,0.660820696335935));
#6601=CARTESIAN_POINT('Ctrl Pts',(9.15949290620382,-20.7415120277891,0.593075062137148));
#6602=CARTESIAN_POINT('Ctrl Pts',(9.18578395639847,-20.7556777898584,0.525325122655411));
#6603=CARTESIAN_POINT('Ctrl Pts',(9.20981183404347,-20.7712663680247,0.456862603466087));
#6604=CARTESIAN_POINT('Ctrl Pts',(9.23145571231611,-20.7882085552331,0.388009033183664));
#6605=CARTESIAN_POINT('Ctrl Pts',(9.25309435428247,-20.8051466436159,0.319172120654451));
#6606=CARTESIAN_POINT('Ctrl Pts',(9.27234995304531,-20.8234375084615,0.249945031381689));
#6607=CARTESIAN_POINT('Ctrl Pts',(9.2891468470743,-20.8429866849445,0.180655744949017));
#6608=CARTESIAN_POINT('Ctrl Pts',(9.30596927096614,-20.8625655745276,0.111261144642447));
#6609=CARTESIAN_POINT('Ctrl Pts',(9.32032544605971,-20.8834063592587,0.041804843379192));
#6610=CARTESIAN_POINT('Ctrl Pts',(9.33218657768053,-20.9053919268366,-0.0273873077118918));
#6611=CARTESIAN_POINT('Ctrl Pts',(9.3401432145608,-20.9201401973571,-0.0738025098018784));
#6612=CARTESIAN_POINT('Ctrl Pts',(9.34697808876498,-20.9354031528252,-0.120098937659683));
#6613=CARTESIAN_POINT('Ctrl Pts',(9.35269438438333,-20.9511407742511,-0.166181422977341));
#6614=CARTESIAN_POINT('Ctrl Pts',(9.36121564506691,-20.9746007881591,-0.234876412977098));
#6615=CARTESIAN_POINT('Ctrl Pts',(9.3675453741578,-20.999706842796,-0.303705335324624));
#6616=CARTESIAN_POINT('Ctrl Pts',(9.3716049858295,-21.0263762358853,-0.372344470076549));
#6617=CARTESIAN_POINT('Ctrl Pts',(9.37565922906612,-21.0530103613389,-0.440892836358829));
#6618=CARTESIAN_POINT('Ctrl Pts',(9.37744916363083,-21.0812035409916,-0.509251242355766));
#6619=CARTESIAN_POINT('Ctrl Pts',(9.37693764066361,-21.1108419111196,-0.577093346533461));
#6620=CARTESIAN_POINT('Ctrl Pts',(9.37642608518874,-21.1404821647871,-0.644939762125091));
#6621=CARTESIAN_POINT('Ctrl Pts',(9.37361270847825,-21.171567548381,-0.712269124556508));
#6622=CARTESIAN_POINT('Ctrl Pts',(9.36850350597585,-21.2039556339764,-0.778761359260748));
#6623=CARTESIAN_POINT('Ctrl Pts',(9.36339553954347,-21.2363358839181,-0.845237507490097));
#6624=CARTESIAN_POINT('Ctrl Pts',(9.35599292530834,-21.2700178752143,-0.910876280136405));
#6625=CARTESIAN_POINT('Ctrl Pts',(9.34634481031159,-21.3048350847771,-0.975374241032964));
#6626=CARTESIAN_POINT('Ctrl Pts',(9.33668203099342,-21.3397052135631,-1.03997023339255));
#6627=CARTESIAN_POINT('Ctrl Pts',(9.32476710728983,-21.3757136242566,-1.10342135481028));
#6628=CARTESIAN_POINT('Ctrl Pts',(9.31069080120018,-21.4126741784787,-1.16544861040113));
#6629=CARTESIAN_POINT('Ctrl Pts',(9.3012481898413,-21.437467909654,-1.20705748594504));
#6630=CARTESIAN_POINT('Ctrl Pts',(9.29083383339552,-21.4626897130814,-1.24802618569427));
#6631=CARTESIAN_POINT('Ctrl Pts',(9.27948472328098,-21.4882800511012,-1.28827884419634));
#6632=CARTESIAN_POINT('Ctrl Pts',(9.26256664691328,-21.5264274731038,-1.34828333297726));
#6633=CARTESIAN_POINT('Ctrl Pts',(9.2436400707703,-21.5661152623663,-1.40722791797283));
#6634=CARTESIAN_POINT('Ctrl Pts',(9.22275033861447,-21.6071891658306,-1.46480935021324));
#6635=CARTESIAN_POINT('Ctrl Pts',(9.20188823106402,-21.6482087531186,-1.52231463670266));
#6636=CARTESIAN_POINT('Ctrl Pts',(9.17906822598555,-21.6906104880492,-1.57845972694475));
#6637=CARTESIAN_POINT('Ctrl Pts',(9.15437367526274,-21.7342109357619,-1.63296134034085));
#6638=CARTESIAN_POINT('Ctrl Pts',(9.12967755518386,-21.7778141543139,-1.68746641735284));
#6639=CARTESIAN_POINT('Ctrl Pts',(9.10310683249362,-21.8226158480044,-1.74032721705642));
#6640=CARTESIAN_POINT('Ctrl Pts',(9.07478121918489,-21.8684079346285,-1.79128851362561));
#6641=CARTESIAN_POINT('Ctrl Pts',(9.04646245869541,-21.9141889427672,-1.8422374811218));
#6642=CARTESIAN_POINT('Ctrl Pts',(9.01638995002209,-21.9609594037198,-1.89128737321232));
#6643=CARTESIAN_POINT('Ctrl Pts',(8.98471606654793,-22.0084931966421,-1.93821939640159));
#6644=CARTESIAN_POINT('Ctrl Pts',(8.95299404144121,-22.0560992369223,-1.98522275230941));
#6645=CARTESIAN_POINT('Ctrl Pts',(8.91966614798735,-22.1044704314653,-2.03010142110779));
#6646=CARTESIAN_POINT('Ctrl Pts',(8.88491325858982,-22.1533686166261,-2.07267852251415));
#6647=CARTESIAN_POINT('Ctrl Pts',(8.86160046430393,-22.1861703016477,-2.10123992341012));
#6648=CARTESIAN_POINT('Ctrl Pts',(8.83764700500886,-22.2192089097494,-2.12876654161632));
#6649=CARTESIAN_POINT('Ctrl Pts',(8.81311307834095,-22.2524115051551,-2.15521684061908));
#6650=CARTESIAN_POINT('Ctrl Pts',(8.77654044482297,-22.3019064910192,-2.19464620327117));
#6651=CARTESIAN_POINT('Ctrl Pts',(8.73857280660773,-22.3525876425948,-2.23203175294834));
#6652=CARTESIAN_POINT('Ctrl Pts',(8.69935947210196,-22.4042406828083,-2.26715077383193));
#6653=CARTESIAN_POINT('Ctrl Pts',(8.66019799335401,-22.4558254169831,-2.30222335328266));
#6654=CARTESIAN_POINT('Ctrl Pts',(8.61979440522145,-22.5083790383233,-2.33503490407258));
#6655=CARTESIAN_POINT('Ctrl Pts',(8.57832444667329,-22.5616647722598,-2.36540131373503));
#6656=CARTESIAN_POINT('Ctrl Pts',(8.53685185268005,-22.6149538925422,-2.39576965320422));
#6657=CARTESIAN_POINT('Ctrl Pts',(8.49431312612197,-22.6689747175642,-2.42369216050347));
#6658=CARTESIAN_POINT('Ctrl Pts',(8.45090606686655,-22.7234740810654,-2.44902900915278));
#6659=CARTESIAN_POINT('Ctrl Pts',(8.40750950908663,-22.7779602595285,-2.47435972805499));
#6660=CARTESIAN_POINT('Ctrl Pts',(8.36324547515667,-22.8329242014082,-2.49710580690364));
#6661=CARTESIAN_POINT('Ctrl Pts',(8.31832753732902,-22.8881044526766,-2.51717642960941));
#6662=CARTESIAN_POINT('Ctrl Pts',(8.27334132802268,-22.9433685732749,-2.53727755796965));
#6663=CARTESIAN_POINT('Ctrl Pts',(8.22769969513748,-22.9988491085934,-2.55469500339245));
#6664=CARTESIAN_POINT('Ctrl Pts',(8.18162632774061,-23.0542831747744,-2.56938903350697));
#6665=CARTESIAN_POINT('Ctrl Pts',(8.15071957567454,-23.0914692333648,-2.57924602402579));
#6666=CARTESIAN_POINT('Ctrl Pts',(8.11961872669561,-23.1286343888246,-2.5878785763622));
#6667=CARTESIAN_POINT('Ctrl Pts',(8.0883919872726,-23.1657010814762,-2.59528770975726));
#6668=CARTESIAN_POINT('Ctrl Pts',(8.04184240259629,-23.2209562627772,-2.60633247743792));
#6669=CARTESIAN_POINT('Ctrl Pts',(7.99482026133714,-23.2768650341225,-2.6147543251795));
#6670=CARTESIAN_POINT('Ctrl Pts',(7.94753828012866,-23.3331765096818,-2.62045518191379));
#6671=CARTESIAN_POINT('Ctrl Pts',(7.90031882466558,-23.3894135188822,-2.62614849982869));
#6672=CARTESIAN_POINT('Ctrl Pts',(7.85284065434047,-23.4460516521555,-2.62912778112528));
#6673=CARTESIAN_POINT('Ctrl Pts',(7.80532548315392,-23.5028275912359,-2.62934454720093));
#6674=CARTESIAN_POINT('Ctrl Pts',(7.75780729234462,-23.5596071384675,-2.62956132705223));
#6675=CARTESIAN_POINT('Ctrl Pts',(7.71025256303128,-23.6165239540305,-2.62701514692949));
#6676=CARTESIAN_POINT('Ctrl Pts',(7.66288608802028,-23.6733092872841,-2.62170927404788));
#6677=CARTESIAN_POINT('Ctrl Pts',(7.61553107238672,-23.7300808824546,-2.61640468481679));
#6678=CARTESIAN_POINT('Ctrl Pts',(7.56836468800612,-23.7867204971482,-2.60834181054537));
#6679=CARTESIAN_POINT('Ctrl Pts',(7.52160755734099,-23.8429626068964,-2.59757579979083));
#6680=CARTESIAN_POINT('Ctrl Pts',(7.47477935977912,-23.89929019991,-2.58679342560759));
#6681=CARTESIAN_POINT('Ctrl Pts',(7.4283621048939,-23.9552185407989,-2.57329990897789));
#6682=CARTESIAN_POINT('Ctrl Pts',(7.38256652431042,-24.0104922266885,-2.55720053492594));
#6683=CARTESIAN_POINT('Ctrl Pts',(7.35184611608344,-24.0475706996133,-2.54640081720705));
#6684=CARTESIAN_POINT('Ctrl Pts',(7.32140521877035,-24.0843548318013,-2.53442952081188));
#6685=CARTESIAN_POINT('Ctrl Pts',(7.29130326403902,-24.1207721297085,-2.52133001886304));
#6686=CARTESIAN_POINT('Ctrl Pts',(7.24643039173222,-24.1750592606718,-2.50180263987787));
#6687=CARTESIAN_POINT('Ctrl Pts',(7.20213366183125,-24.2293945150359,-2.47959273545138));
#6688=CARTESIAN_POINT('Ctrl Pts',(7.15863608400191,-24.2835210642857,-2.45474630344363));
#6689=CARTESIAN_POINT('Ctrl Pts',(7.11519602741874,-24.3375760365254,-2.42993272838569));
#6690=CARTESIAN_POINT('Ctrl Pts',(7.07255348352948,-24.3914223195744,-2.40248965698964));
#6691=CARTESIAN_POINT('Ctrl Pts',(7.0309206233938,-24.4448021047863,-2.37251384629869));
#6692=CARTESIAN_POINT('Ctrl Pts',(6.98928511746054,-24.4981852823212,-2.34253613062386));
#6693=CARTESIAN_POINT('Ctrl Pts',(6.94865986736745,-24.551101361191,-2.31002556527924));
#6694=CARTESIAN_POINT('Ctrl Pts',(6.90924021764144,-24.603298592727,-2.27512786406314));
#6695=CARTESIAN_POINT('Ctrl Pts',(6.8698301047165,-24.6554831961799,-2.24023860565251));
#6696=CARTESIAN_POINT('Ctrl Pts',(6.83162539079327,-24.7069487880225,-2.20296372939517));
#6697=CARTESIAN_POINT('Ctrl Pts',(6.79479820350458,-24.7574578422892,-2.16349342564679));
#6698=CARTESIAN_POINT('Ctrl Pts',(6.75791504199586,-24.8080436660604,-2.12396313036418));
#6699=CARTESIAN_POINT('Ctrl Pts',(6.72241390399149,-24.8576695839296,-2.08223120813761));
#6700=CARTESIAN_POINT('Ctrl Pts',(6.68843935594901,-24.9061183934996,-2.03852710839605));
#6701=CARTESIAN_POINT('Ctrl Pts',(6.66564868549808,-24.9386186301846,-2.0092096989836));
#6702=CARTESIAN_POINT('Ctrl Pts',(6.64354436967967,-24.9705896348024,-1.97900561592636));
#6703=CARTESIAN_POINT('Ctrl Pts',(6.62216201968439,-25.0019726665679,-1.94799199564959));
#6704=CARTESIAN_POINT('Ctrl Pts',(6.5902874298272,-25.0487552356599,-1.90176010689427));
#6705=CARTESIAN_POINT('Ctrl Pts',(6.5599562245426,-25.0950274906273,-1.8533173942581));
#6706=CARTESIAN_POINT('Ctrl Pts',(6.53134655267294,-25.1405585033634,-1.80284481408909));
#6707=CARTESIAN_POINT('Ctrl Pts',(6.50277471426566,-25.186029305837,-1.75243897891707));
#6708=CARTESIAN_POINT('Ctrl Pts',(6.47592025032039,-25.2307603366803,-1.70000899168558));
#6709=CARTESIAN_POINT('Ctrl Pts',(6.45093216107982,-25.2745302589353,-1.64577768116459));
#6710=CARTESIAN_POINT('Ctrl Pts',(6.42594248382858,-25.3183029627997,-1.59154292420563));
#6711=CARTESIAN_POINT('Ctrl Pts',(6.40281972658714,-25.3611139727102,-1.53550708982158));
#6712=CARTESIAN_POINT('Ctrl Pts',(6.38167917697755,-25.4027577608735,-1.47792947798907));
#6713=CARTESIAN_POINT('Ctrl Pts',(6.36054374190388,-25.4443914741496,-1.4203657959157));
#6714=CARTESIAN_POINT('Ctrl Pts',(6.34138975060389,-25.4848581261575,-1.36126166406147));
#6715=CARTESIAN_POINT('Ctrl Pts',(6.3242948958368,-25.5239747129312,-1.30090464504799));
#6716=CARTESIAN_POINT('Ctrl Pts',(6.30717405833167,-25.563150753619,-1.24045588845407));
#6717=CARTESIAN_POINT('Ctrl Pts',(6.29211870526331,-25.6009722920517,-1.17875107963611));
#6718=CARTESIAN_POINT('Ctrl Pts',(6.27916713501913,-25.6372834797305,-1.11609838715443));
#6719=CARTESIAN_POINT('Ctrl Pts',(6.27047901446228,-25.661641605438,-1.07406995853689));
#6720=CARTESIAN_POINT('Ctrl Pts',(6.26273674776036,-25.6853206771323,-1.03161537789568));
#6721=CARTESIAN_POINT('Ctrl Pts',(6.25594179788806,-25.7082816695101,-0.988830267143717));
#6722=CARTESIAN_POINT('Ctrl Pts',(6.24581259130752,-25.7425095357137,-0.925050661183071));
#6723=CARTESIAN_POINT('Ctrl Pts',(6.23792098047084,-25.7758262847861,-0.859969813685577));
#6724=CARTESIAN_POINT('Ctrl Pts',(6.23235398477746,-25.808053602229,-0.793867798863225));
#6725=CARTESIAN_POINT('Ctrl Pts',(6.22679435088548,-25.8402383022309,-0.727853197420082));
#6726=CARTESIAN_POINT('Ctrl Pts',(6.22355339753122,-25.871336066378,-0.660820696336077));
#6727=CARTESIAN_POINT('Ctrl Pts',(6.22267583801938,-25.9011857678037,-0.593075062137264));
#6728=CARTESIAN_POINT('Ctrl Pts',(6.22179822273801,-25.9310373661991,-0.525325122655538));
#6729=CARTESIAN_POINT('Ctrl Pts',(6.22328438861643,-25.9596404077219,-0.456862603466225));
#6730=CARTESIAN_POINT('Ctrl Pts',(6.2271348139982,-25.9868556497466,-0.388009033183813));
#6731=CARTESIAN_POINT('Ctrl Pts',(6.23098430784604,-26.0140643075841,-0.319172120654854));
#6732=CARTESIAN_POINT('Ctrl Pts',(6.23719686207813,-26.0398855777006,-0.249945031382356));
#6733=CARTESIAN_POINT('Ctrl Pts',(6.24572849852092,-26.0642067028758,-0.18065574494994));
#6734=CARTESIAN_POINT('Ctrl Pts',(6.25427310233184,-26.0885647941109,-0.111261144643501));
#6735=CARTESIAN_POINT('Ctrl Pts',(6.26514366379693,-26.1114179988086,-0.0418048433803723));
#6736=CARTESIAN_POINT('Ctrl Pts',(6.27825315802551,-26.1326828238988,0.0273873077105849));
#6737=CARTESIAN_POINT('Ctrl Pts',(6.2870472165181,-26.1469476088262,0.0738025098010098));
#6738=CARTESIAN_POINT('Ctrl Pts',(6.29684788658832,-26.1604982612529,0.120098937659253));
#6739=CARTESIAN_POINT('Ctrl Pts',(6.30761891872917,-26.1733175291869,0.166181422977344));
#6740=CARTESIAN_POINT('Ctrl Pts',(6.32367525640489,-26.1924271643652,0.234876412977188));
#6741=CARTESIAN_POINT('Ctrl Pts',(6.34225287296385,-26.2104618978755,0.303705335324803));
#6742=CARTESIAN_POINT('Ctrl Pts',(6.36331943904686,-26.2273123212574,0.372344470076813));
#6743=CARTESIAN_POINT('Ctrl Pts',(6.38435814667899,-26.2441404616202,0.440892836359177));
#6744=CARTESIAN_POINT('Ctrl Pts',(6.40787918918932,-26.2597871802507,0.509251242356202));
#6745=CARTESIAN_POINT('Ctrl Pts',(6.43380253213062,-26.2741633734305,0.577093346533977));
#6746=CARTESIAN_POINT('Ctrl Pts',(6.45972752251878,-26.2885404802276,0.644939762125664));
#6747=CARTESIAN_POINT('Ctrl Pts',(6.48805494275271,-26.3016467163228,0.712269124557124));
#6748=CARTESIAN_POINT('Ctrl Pts',(6.51865844890955,-26.3134160599604,0.778761359261416));
#6749=CARTESIAN_POINT('Ctrl Pts',(6.54925455115611,-26.3251825562391,0.845237507490585));
#6750=CARTESIAN_POINT('Ctrl Pts',(6.58212531838614,-26.3356126999051,0.910876280136723));
#6751=CARTESIAN_POINT('Ctrl Pts',(6.61710196385465,-26.3446657920006,0.975374241033112));
#6752=CARTESIAN_POINT('Ctrl Pts',(6.65213177087563,-26.3537326440329,1.03997023339268));
#6753=CARTESIAN_POINT('Ctrl Pts',(6.68927343113795,-26.3614182227682,1.10342135481039));
#6754=CARTESIAN_POINT('Ctrl Pts',(6.72832036307706,-26.3677080612142,1.16544861040121));
#6755=CARTESIAN_POINT('Ctrl Pts',(6.7545136698089,-26.371927385487,1.20705748594509));
#6756=CARTESIAN_POINT('Ctrl Pts',(6.78156357052916,-26.3755191899546,1.24802618569429));
#6757=CARTESIAN_POINT('Ctrl Pts',(6.80940000840295,-26.3784857412949,1.28827884419633));
#6758=CARTESIAN_POINT('Ctrl Pts',(6.85089568313002,-26.3829079683787,1.34828333297733));
#6759=CARTESIAN_POINT('Ctrl Pts',(6.89472960492293,-26.3863609672634,1.40722791797297));
#6760=CARTESIAN_POINT('Ctrl Pts',(6.94074551483355,-26.3888068802704,1.46480935021343));
#6761=CARTESIAN_POINT('Ctrl Pts',(6.98670057325275,-26.3912495587992,1.52231463670264));
#6762=CARTESIAN_POINT('Ctrl Pts',(7.03483155540622,-26.392687722152,1.57845972694453));
#6763=CARTESIAN_POINT('Ctrl Pts',(7.08493792610307,-26.3931018377474,1.63296134034044));
#6764=CARTESIAN_POINT('Ctrl Pts',(7.13504748109524,-26.3935159796601,1.68746641735244));
#6765=CARTESIAN_POINT('Ctrl Pts',(7.18713224730889,-26.3929059056587,1.74032721705603));
#6766=CARTESIAN_POINT('Ctrl Pts',(7.24095216427203,-26.3912712482677,1.79128851362524));
#6767=CARTESIAN_POINT('Ctrl Pts',(7.29475906057568,-26.3896369863495,1.84223748112135));
#6768=CARTESIAN_POINT('Ctrl Pts',(7.3502997222439,-26.3869786603592,1.89128737321179));
#6769=CARTESIAN_POINT('Ctrl Pts',(7.40730213618982,-26.3833151690952,1.93821939640099));
#6770=CARTESIAN_POINT('Ctrl Pts',(7.46439118899938,-26.3796461096334,1.98522275230886));
#6771=CARTESIAN_POINT('Ctrl Pts',(7.52294581901199,-26.3749689045192,2.03010142110728));
#6772=CARTESIAN_POINT('Ctrl Pts',(7.582669334259,-26.3693211120265,2.07267852251368));
#6773=CARTESIAN_POINT('Ctrl Pts',(7.62273282391778,-26.3655324824525,2.10123992340982));
#6774=CARTESIAN_POINT('Ctrl Pts',(7.66332182748728,-26.3613074822452,2.12876654161618));
#6775=CARTESIAN_POINT('Ctrl Pts',(7.7043430819144,-26.3566617761991,2.15521684061908));
#6776=CARTESIAN_POINT('Ctrl Pts',(7.76549331379184,-26.3497364394213,2.19464620327127));
#6777=CARTESIAN_POINT('Ctrl Pts',(7.8283682976571,-26.3421960759929,2.23203175294854));
#6778=CARTESIAN_POINT('Ctrl Pts',(7.89270780991775,-26.3340628522506,2.2671507738322));
#6779=CARTESIAN_POINT('Ctrl Pts',(7.95696223953461,-26.3259403838925,2.30222335328292));
#6780=CARTESIAN_POINT('Ctrl Pts',(8.02267680474233,-26.3172266608357,2.33503490407283));
#6781=CARTESIAN_POINT('Ctrl Pts',(8.08955858326471,-26.3079554902074,2.36540131373527));
#6782=CARTESIAN_POINT('Ctrl Pts',(8.15644461217124,-26.2986837303896,2.39576965320444));
#6783=CARTESIAN_POINT('Ctrl Pts',(8.22449738225272,-26.2888545250567,2.42369216050368));
#6784=CARTESIAN_POINT('Ctrl Pts',(8.29339874516257,-26.2785125907885,2.44902900915297));
#6785=CARTESIAN_POINT('Ctrl Pts',(8.36228343875657,-26.2681731585459,2.47435972805512));
#6786=CARTESIAN_POINT('Ctrl Pts',(8.43201562568134,-26.2573213516284,2.49710580690372));
#6787=CARTESIAN_POINT('Ctrl Pts',(8.50226209398065,-26.2460114020183,2.51717642960944));
#6788=CARTESIAN_POINT('Ctrl Pts',(8.57261533098984,-26.2346842622382,2.53727755796968));
#6789=CARTESIAN_POINT('Ctrl Pts',(8.64348370043378,-26.2228977163486,2.55469500339248));
#6790=CARTESIAN_POINT('Ctrl Pts',(8.71452769368014,-26.2107140428356,2.569389033507));
#6791=CARTESIAN_POINT('Ctrl Pts',(8.76218514111895,-26.202541039693,2.5792460240258));
#6792=CARTESIAN_POINT('Ctrl Pts',(8.80992153437213,-26.1941894921279,2.58787857636221));
#6793=CARTESIAN_POINT('Ctrl Pts',(8.85763560155417,-26.1856796888361,2.59528770975726));
#6794=CARTESIAN_POINT('Ctrl Pts',(8.92876278459006,-26.1729941566213,2.60633247743796));
#6795=CARTESIAN_POINT('Ctrl Pts',(9.00069227149935,-26.1602261734231,2.61475432517956));
#6796=CARTESIAN_POINT('Ctrl Pts',(9.07310043046284,-26.1474345143349,2.62045518191386));
#6797=CARTESIAN_POINT('Ctrl Pts',(9.14541283679517,-26.1346597709511,2.62614849982877));
#6798=CARTESIAN_POINT('Ctrl Pts',(9.21820198419582,-26.1218615359609,2.62912778112534));
#6799=CARTESIAN_POINT('Ctrl Pts',(9.29112897535694,-26.1091001601884,2.62934454720093));
#6800=CARTESIAN_POINT('Ctrl Pts',(9.36406060107956,-26.0963379734214,2.62956132705217));
#6801=CARTESIAN_POINT('Ctrl Pts',(9.43712937391635,-26.0836127775475,2.62701514692937));
#6802=CARTESIAN_POINT('Ctrl Pts',(9.5099901525818,-26.070984873527,2.6217092740477));
#6803=CARTESIAN_POINT('Ctrl Pts',(9.5828333040297,-26.0583600245769,2.61640468481655));
#6804=CARTESIAN_POINT('Ctrl Pts',(9.65546784140534,-26.0458325448455,2.60834181054505));
#6805=CARTESIAN_POINT('Ctrl Pts',(9.7275535025424,-26.0334607367555,2.59757579979043));
#6806=CARTESIAN_POINT('Ctrl Pts',(9.79974872780703,-26.0210701245603,2.58679342560712));
#6807=CARTESIAN_POINT('Ctrl Pts',(9.8713927192509,-26.0088357731002,2.57329990897737));
#6808=CARTESIAN_POINT('Ctrl Pts',(9.94215892568377,-25.9968124798787,2.55720053492538));
#6809=CARTESIAN_POINT('Ctrl Pts',(9.9896300292828,-25.988747062402,2.54640081720663));
#6810=CARTESIAN_POINT('Ctrl Pts',(10.0367064708695,-25.980776538109,2.53442952081165));
#6811=CARTESIAN_POINT('Ctrl Pts',(10.0832957533592,-25.9729161295619,2.52133001886304));
#6812=CARTESIAN_POINT('Ctrl Pts',(10.1527462240253,-25.9611986476851,2.50180263987788));
#6813=CARTESIAN_POINT('Ctrl Pts',(10.2219502995762,-25.9500041814683,2.47959273545139));
#6814=CARTESIAN_POINT('Ctrl Pts',(10.2905740551603,-25.9393974486899,2.45474630344365));
#6815=CARTESIAN_POINT('Ctrl Pts',(10.3591070626124,-25.9288047422669,2.42993272838573));
#6816=CARTESIAN_POINT('Ctrl Pts',(10.4270605835768,-25.9187983575013,2.40248965698969));
#6817=CARTESIAN_POINT('Ctrl Pts',(10.4941052636867,-25.9094331355976,2.37251384629875));
#6818=CARTESIAN_POINT('Ctrl Pts',(10.5611542045333,-25.9000673185274,2.3425361306239));
#6819=CARTESIAN_POINT('Ctrl Pts',(10.6272934981498,-25.8913428593466,2.31002556527924));
#6820=CARTESIAN_POINT('Ctrl Pts',(10.6922074515303,-25.8833030570436,2.2751278640631));
#6821=CARTESIAN_POINT('Ctrl Pts',(10.7571057002693,-25.875265199811,2.24023860565252));
#6822=CARTESIAN_POINT('Ctrl Pts',(10.8207785671873,-25.8679117429305,2.20296372939525));
#6823=CARTESIAN_POINT('Ctrl Pts',(10.8829342849477,-25.8612729903219,2.16349342564694));
#6824=CARTESIAN_POINT('Ctrl Pts',(10.9451844741592,-25.854624147369,2.12396313036433));
#6825=CARTESIAN_POINT('Ctrl Pts',(11.0059123487223,-25.8486922189286,2.08223120813775));
#6826=CARTESIAN_POINT('Ctrl Pts',(11.0648575226142,-25.8434938020267,2.03852710839618));
#6827=CARTESIAN_POINT('Ctrl Pts',(11.104398888438,-25.8400066207894,2.0092096989837));
#6828=CARTESIAN_POINT('Ctrl Pts',(11.1431387485308,-25.8368492240663,1.97900561592641));
#6829=CARTESIAN_POINT('Ctrl Pts',(11.1810084262852,-25.8340230816606,1.94799199564959));
#6830=CARTESIAN_POINT('Ctrl Pts',(11.2374606145019,-25.829810161655,1.90176010689413));
#6831=CARTESIAN_POINT('Ctrl Pts',(11.2926991654365,-25.8266786948348,1.8533173942578));
#6832=CARTESIAN_POINT('Ctrl Pts',(11.3464350150611,-25.8246674985698,1.80284481408862));
#6833=CARTESIAN_POINT('Ctrl Pts',(11.4000998043371,-25.8226589619131,1.7524389789167));
#6834=CARTESIAN_POINT('Ctrl Pts',(11.4522652453575,-25.8217678293531,1.7000089916853));
#6835=CARTESIAN_POINT('Ctrl Pts',(11.5026651545722,-25.8220124704063,1.64577768116442));
#6836=CARTESIAN_POINT('Ctrl Pts',(11.5530682667367,-25.8222571270065,1.59154292420547));
#6837=CARTESIAN_POINT('Ctrl Pts',(11.6017050675015,-25.8236377367852,1.53550708982144));
#6838=CARTESIAN_POINT('Ctrl Pts',(11.6483399207655,-25.8261513778549,1.47792947798895));
#6839=CARTESIAN_POINT('Ctrl Pts',(11.6949634916533,-25.8286644107992,1.42036579591568));
#6840=CARTESIAN_POINT('Ctrl Pts',(11.7395856359481,-25.8323098937535,1.36126166406155));
#6841=CARTESIAN_POINT('Ctrl Pts',(11.782009021187,-25.837063608638,1.30090464504817));
#6842=CARTESIAN_POINT('Ctrl Pts',(11.8244968863949,-25.8418245487684,1.24045588845423));
#6843=CARTESIAN_POINT('Ctrl Pts',(11.864778976022,-25.8476969997645,1.17875107963624));
#6844=CARTESIAN_POINT('Ctrl Pts',(11.9027011721156,-25.8546362047536,1.11609838715453));
#6845=CARTESIAN_POINT('Ctrl Pts',(11.9281399880453,-25.859291134494,1.07406995853695));
#6846=CARTESIAN_POINT('Ctrl Pts',(11.9525177990215,-25.8644256706944,1.03161537789571));
#6847=CARTESIAN_POINT('Ctrl Pts',(11.975800076653,-25.8700215676765,0.988830267143717));
#6848=CARTESIAN_POINT('Ctrl Pts',(12.0105068815926,-25.8783633505592,0.925050661183495));
#6849=CARTESIAN_POINT('Ctrl Pts',(12.043305838079,-25.888187389634,0.859969813686448));
#6850=CARTESIAN_POINT('Ctrl Pts',(12.0739990115269,-25.8994798886622,0.793867798864551));
#6851=CARTESIAN_POINT('Ctrl Pts',(12.1046515962878,-25.9107574544769,0.727853197421398));
#6852=CARTESIAN_POINT('Ctrl Pts',(12.1332035267172,-25.9234995886132,0.660820696337378));
#6853=CARTESIAN_POINT('Ctrl Pts',(12.1594929062032,-25.9376644504955,0.593075062138549));
#6854=CARTESIAN_POINT('Ctrl Pts',(12.1857839563979,-25.9518302125647,0.525325122656871));
#6855=CARTESIAN_POINT('Ctrl Pts',(12.2098118340429,-25.967418790731,0.456862603467601));
#6856=CARTESIAN_POINT('Ctrl Pts',(12.2314557123156,-25.9843609779393,0.388009033185234));
#6857=CARTESIAN_POINT('Ctrl Pts',(12.253094354282,-26.0012990663221,0.319172120656097));
#6858=CARTESIAN_POINT('Ctrl Pts',(12.2723499530448,-26.0195899311677,0.249945031383417));
#6859=CARTESIAN_POINT('Ctrl Pts',(12.2891468470738,-26.0391391076507,0.180655744950817));
#6860=CARTESIAN_POINT('Ctrl Pts',(12.3059692709657,-26.0587179972338,0.111261144644251));
#6861=CARTESIAN_POINT('Ctrl Pts',(12.3203254460593,-26.0795587819648,0.0418048433809942));
#6862=CARTESIAN_POINT('Ctrl Pts',(12.3321865776802,-26.1015443495427,-0.0273873077100924));
#6863=CARTESIAN_POINT('Ctrl Pts',(12.3401432145606,-26.1162926200634,-0.0738025098006832));
#6864=CARTESIAN_POINT('Ctrl Pts',(12.3469780887649,-26.1315555755317,-0.120098937659091));
#6865=CARTESIAN_POINT('Ctrl Pts',(12.3526943843833,-26.1472931969577,-0.166181422977345));
#6866=CARTESIAN_POINT('Ctrl Pts',(12.3612156450669,-26.1707532108657,-0.234876412977034));
#6867=CARTESIAN_POINT('Ctrl Pts',(12.3675453741578,-26.1958592655026,-0.303705335324481));
#6868=CARTESIAN_POINT('Ctrl Pts',(12.3716049858295,-26.2225286585919,-0.372344470076339));
#6869=CARTESIAN_POINT('Ctrl Pts',(12.3756592290661,-26.2491627840458,-0.440892836359306));
#6870=CARTESIAN_POINT('Ctrl Pts',(12.3774491636308,-26.2773559636987,-0.509251242356935));
#6871=CARTESIAN_POINT('Ctrl Pts',(12.3769376406636,-26.3069943338271,-0.577093346535299));
#6872=CARTESIAN_POINT('Ctrl Pts',(12.3764260851887,-26.3366345874946,-0.644939762127014));
#6873=CARTESIAN_POINT('Ctrl Pts',(12.3736127084781,-26.3677199710885,-0.712269124558506));
#6874=CARTESIAN_POINT('Ctrl Pts',(12.3685035059757,-26.4001080566841,-0.778761359262821));
#6875=CARTESIAN_POINT('Ctrl Pts',(12.3633955395432,-26.4324883066258,-0.845237507492121));
#6876=CARTESIAN_POINT('Ctrl Pts',(12.3559929253081,-26.466170297922,-0.910876280138376));
#6877=CARTESIAN_POINT('Ctrl Pts',(12.3463448103113,-26.5009875074848,-0.975374241034882));
#6878=CARTESIAN_POINT('Ctrl Pts',(12.3366820309931,-26.5358576362707,-1.03997023339422));
#6879=CARTESIAN_POINT('Ctrl Pts',(12.3247671072895,-26.5718660469641,-1.10342135481171));
#6880=CARTESIAN_POINT('Ctrl Pts',(12.3106908011999,-26.6088266011861,-1.16544861040232));
#6881=CARTESIAN_POINT('Ctrl Pts',(12.3012481898411,-26.6336203323612,-1.20705748594582));
#6882=CARTESIAN_POINT('Ctrl Pts',(12.2908338333954,-26.6588421357883,-1.24802618569465));
#6883=CARTESIAN_POINT('Ctrl Pts',(12.279484723281,-26.6844324738078,-1.28827884419634));
#6884=CARTESIAN_POINT('Ctrl Pts',(12.2625666469133,-26.7225798958103,-1.34828333297698));
#6885=CARTESIAN_POINT('Ctrl Pts',(12.2436400707704,-26.7622676850726,-1.40722791797229));
#6886=CARTESIAN_POINT('Ctrl Pts',(12.2227503386147,-26.8033415885367,-1.46480935021245));
#6887=CARTESIAN_POINT('Ctrl Pts',(12.2018882310643,-26.8443611758246,-1.52231463670186));
#6888=CARTESIAN_POINT('Ctrl Pts',(12.1790682259859,-26.8867629107552,-1.57845972694394));
#6889=CARTESIAN_POINT('Ctrl Pts',(12.1543736752631,-26.9303633584679,-1.63296134034003));
#6890=CARTESIAN_POINT('Ctrl Pts',(12.1296775551842,-26.9739665770198,-1.68746641735199));
#6891=CARTESIAN_POINT('Ctrl Pts',(12.103106832494,-27.0187682707103,-1.74032721705555));
#6892=CARTESIAN_POINT('Ctrl Pts',(12.0747812191854,-27.0645603573343,-1.79128851362472));
#6893=CARTESIAN_POINT('Ctrl Pts',(12.0464624586959,-27.110341365473,-1.84223748112084));
#6894=CARTESIAN_POINT('Ctrl Pts',(12.0163899500227,-27.1571118264255,-1.89128737321128));
#6895=CARTESIAN_POINT('Ctrl Pts',(11.9847160665486,-27.2046456193477,-1.93821939640049));
#6896=CARTESIAN_POINT('Ctrl Pts',(11.9529940414419,-27.2522516596279,-1.98522275230842));
#6897=CARTESIAN_POINT('Ctrl Pts',(11.919666147988,-27.300622854171,-2.0301014211069));
#6898=CARTESIAN_POINT('Ctrl Pts',(11.8849132585904,-27.3495210393319,-2.07267852251336));
#6899=CARTESIAN_POINT('Ctrl Pts',(11.8616004643043,-27.3823227243537,-2.10123992340961));
#6900=CARTESIAN_POINT('Ctrl Pts',(11.8376470050091,-27.4153613324557,-2.12876654161608));
#6901=CARTESIAN_POINT('Ctrl Pts',(11.8131130783409,-27.4485639278618,-2.15521684061907));
#6902=CARTESIAN_POINT('Ctrl Pts',(11.776540444823,-27.4980589137259,-2.19464620327115));
#6903=CARTESIAN_POINT('Ctrl Pts',(11.7385728066077,-27.5487400653014,-2.23203175294831));
#6904=CARTESIAN_POINT('Ctrl Pts',(11.699359472102,-27.6003931055149,-2.26715077383189));
#6905=CARTESIAN_POINT('Ctrl Pts',(11.6601979933545,-27.6519778396891,-2.30222335328218));
#6906=CARTESIAN_POINT('Ctrl Pts',(11.6197944052225,-27.7045314610286,-2.33503490407172));
#6907=CARTESIAN_POINT('Ctrl Pts',(11.5783244466749,-27.7578171949644,-2.36540131373386));
#6908=CARTESIAN_POINT('Ctrl Pts',(11.5368518526816,-27.8111063152468,-2.39576965320312));
#6909=CARTESIAN_POINT('Ctrl Pts',(11.4943131261236,-27.8651271402688,-2.42369216050245));
#6910=CARTESIAN_POINT('Ctrl Pts',(11.4509060668681,-27.91962650377,-2.44902900915183));
#6911=CARTESIAN_POINT('Ctrl Pts',(11.4075095090882,-27.9741126822331,-2.4743597280541));
#6912=CARTESIAN_POINT('Ctrl Pts',(11.3632454751583,-28.0290766241127,-2.49710580690281));
#6913=CARTESIAN_POINT('Ctrl Pts',(11.3183275373307,-28.0842568753811,-2.51717642960864));
#6914=CARTESIAN_POINT('Ctrl Pts',(11.2733413280244,-28.1395209959794,-2.53727755796891));
#6915=CARTESIAN_POINT('Ctrl Pts',(11.2276996951393,-28.1950015312977,-2.55469500339175));
#6916=CARTESIAN_POINT('Ctrl Pts',(11.1816263277426,-28.2504355974787,-2.56938903350633));
#6917=CARTESIAN_POINT('Ctrl Pts',(11.1507195756758,-28.2876216560698,-2.57924602402541));
#6918=CARTESIAN_POINT('Ctrl Pts',(11.1196187266963,-28.3247868115304,-2.58787857636204));
#6919=CARTESIAN_POINT('Ctrl Pts',(11.0883919872726,-28.3618535041829,-2.59528770975725));
#6920=CARTESIAN_POINT('Ctrl Pts',(11.0418424025962,-28.417108685484,-2.60633247743792));
#6921=CARTESIAN_POINT('Ctrl Pts',(10.994820261337,-28.4730174568294,-2.61475432517951));
#6922=CARTESIAN_POINT('Ctrl Pts',(10.9475382801284,-28.5293289323887,-2.6204551819138));
#6923=CARTESIAN_POINT('Ctrl Pts',(10.9003188246655,-28.5855659415888,-2.62614849982868));
#6924=CARTESIAN_POINT('Ctrl Pts',(10.8528406543406,-28.642204074862,-2.62912778112526));
#6925=CARTESIAN_POINT('Ctrl Pts',(10.8053254831542,-28.6989800139423,-2.62934454720093));
#6926=CARTESIAN_POINT('Ctrl Pts',(10.7578072923449,-28.7557595611739,-2.62956132705223));
#6927=CARTESIAN_POINT('Ctrl Pts',(10.7102525630315,-28.8126763767369,-2.6270151469295));
#6928=CARTESIAN_POINT('Ctrl Pts',(10.6628860880205,-28.8694617099905,-2.62170927404791));
#6929=CARTESIAN_POINT('Ctrl Pts',(10.6155310723873,-28.9262333051604,-2.61640468481687));
#6930=CARTESIAN_POINT('Ctrl Pts',(10.5683646880072,-28.9828729198536,-2.60834181054555));
#6931=CARTESIAN_POINT('Ctrl Pts',(10.5216075573424,-29.0391150296013,-2.59757579979117));
#6932=CARTESIAN_POINT('Ctrl Pts',(10.4747793597805,-29.0954426226149,-2.58679342560797));
#6933=CARTESIAN_POINT('Ctrl Pts',(10.4283621048952,-29.1513709635039,-2.57329990897831));
#6934=CARTESIAN_POINT('Ctrl Pts',(10.3825665243117,-29.2066446493936,-2.55720053492641));
#6935=CARTESIAN_POINT('Ctrl Pts',(10.3518461160843,-29.2437231223189,-2.54640081720739));
#6936=CARTESIAN_POINT('Ctrl Pts',(10.3214052187707,-29.2805072545074,-2.53442952081207));
#6937=CARTESIAN_POINT('Ctrl Pts',(10.291303264039,-29.3169245524152,-2.52133001886304));
#6938=CARTESIAN_POINT('Ctrl Pts',(10.2464303917322,-29.3712116833784,-2.50180263987789));
#6939=CARTESIAN_POINT('Ctrl Pts',(10.2021336618313,-29.4255469377425,-2.47959273545141));
#6940=CARTESIAN_POINT('Ctrl Pts',(10.158636084002,-29.4796734869922,-2.45474630344369));
#6941=CARTESIAN_POINT('Ctrl Pts',(10.1151960274185,-29.5337284592323,-2.4299327283856));
#6942=CARTESIAN_POINT('Ctrl Pts',(10.072553483529,-29.5875747422816,-2.40248965698937));
#6943=CARTESIAN_POINT('Ctrl Pts',(10.0309206233931,-29.6409545274939,-2.3725138462982));
#6944=CARTESIAN_POINT('Ctrl Pts',(9.98928511745983,-29.6943377050287,-2.34253613062334));
#6945=CARTESIAN_POINT('Ctrl Pts',(9.94865986736672,-29.7472537838986,-2.31002556527867));
#6946=CARTESIAN_POINT('Ctrl Pts',(9.90924021764072,-29.7994510154346,-2.27512786406253));
#6947=CARTESIAN_POINT('Ctrl Pts',(9.86983010471572,-29.8516356188876,-2.24023860565181));
#6948=CARTESIAN_POINT('Ctrl Pts',(9.83162539079244,-29.9031012107303,-2.20296372939438));
#6949=CARTESIAN_POINT('Ctrl Pts',(9.79479820350371,-29.953610264997,-2.1634934256459));
#6950=CARTESIAN_POINT('Ctrl Pts',(9.757915041995,-30.0041960887682,-2.12396313036324));
#6951=CARTESIAN_POINT('Ctrl Pts',(9.72241390399064,-30.0538220066374,-2.08223120813662));
#6952=CARTESIAN_POINT('Ctrl Pts',(9.68843935594817,-30.1022708162074,-2.03852710839501));
#6953=CARTESIAN_POINT('Ctrl Pts',(9.66564868549753,-30.134771052892,-2.00920969898289));
#6954=CARTESIAN_POINT('Ctrl Pts',(9.64354436967938,-30.1667420575094,-1.97900561592599));
#6955=CARTESIAN_POINT('Ctrl Pts',(9.62216201968436,-30.1981250892746,-1.94799199564958));
#6956=CARTESIAN_POINT('Ctrl Pts',(9.59028742982723,-30.2449076583664,-1.90176010689435));
#6957=CARTESIAN_POINT('Ctrl Pts',(9.55995622454268,-30.2911799133338,-1.85331739425826));
#6958=CARTESIAN_POINT('Ctrl Pts',(9.53134655267306,-30.3367109260699,-1.80284481408935));
#6959=CARTESIAN_POINT('Ctrl Pts',(9.50277471426597,-30.3821817285431,-1.75243897891767));
#6960=CARTESIAN_POINT('Ctrl Pts',(9.47592025032086,-30.4269127593862,-1.70000899168654));
#6961=CARTESIAN_POINT('Ctrl Pts',(9.45093216108043,-30.4706826816409,-1.64577768116595));
#6962=CARTESIAN_POINT('Ctrl Pts',(9.42594248382916,-30.5144553855053,-1.59154292420704));
#6963=CARTESIAN_POINT('Ctrl Pts',(9.4028197265877,-30.5572663954157,-1.53550708982303));
#6964=CARTESIAN_POINT('Ctrl Pts',(9.38167917697807,-30.598910183579,-1.47792947799057));
#6965=CARTESIAN_POINT('Ctrl Pts',(9.36054374190446,-30.640543896855,-1.42036579591748));
#6966=CARTESIAN_POINT('Ctrl Pts',(9.34138975060452,-30.6810105488628,-1.36126166406354));
#6967=CARTESIAN_POINT('Ctrl Pts',(9.32429489583745,-30.7201271356363,-1.30090464505035));
#6968=CARTESIAN_POINT('Ctrl Pts',(9.30717405833223,-30.7593031763242,-1.24045588845638));
#6969=CARTESIAN_POINT('Ctrl Pts',(9.2921187052638,-30.797124714757,-1.17875107963836));
#6970=CARTESIAN_POINT('Ctrl Pts',(9.27916713501956,-30.8334359024359,-1.11609838715662));
#6971=CARTESIAN_POINT('Ctrl Pts',(9.27047901446252,-30.8577940281439,-1.07406995853836));
#6972=CARTESIAN_POINT('Ctrl Pts',(9.26273674776045,-30.8814730998386,-1.03161537789642));
#6973=CARTESIAN_POINT('Ctrl Pts',(9.25594179788803,-30.9044340922168,-0.988830267143717));
#6974=CARTESIAN_POINT('Ctrl Pts',(9.24581259130754,-30.9386619584202,-0.925050661183348));
#6975=CARTESIAN_POINT('Ctrl Pts',(9.23792098047089,-30.9719787074924,-0.859969813686147));
#6976=CARTESIAN_POINT('Ctrl Pts',(9.23235398477751,-31.0042060249353,-0.793867798864092));
#6977=CARTESIAN_POINT('Ctrl Pts',(9.22679435088552,-31.0363907249372,-0.727853197420999));
#6978=CARTESIAN_POINT('Ctrl Pts',(9.22355339753123,-31.0674884890842,-0.660820696337054));
#6979=CARTESIAN_POINT('Ctrl Pts',(9.22267583801937,-31.09733819051,-0.593075062138292));
#6980=CARTESIAN_POINT('Ctrl Pts',(9.22179822273798,-31.1271897889054,-0.525325122656501));
#6981=CARTESIAN_POINT('Ctrl Pts',(9.22328438861637,-31.1557928304282,-0.456862603467119));
#6982=CARTESIAN_POINT('Ctrl Pts',(9.22713481399813,-31.1830080724529,-0.388009033184638));
#6983=CARTESIAN_POINT('Ctrl Pts',(9.23098430784596,-31.2102167302905,-0.319172120655617));
#6984=CARTESIAN_POINT('Ctrl Pts',(9.23719686207803,-31.236038000407,-0.249945031383046));
#6985=CARTESIAN_POINT('Ctrl Pts',(9.24572849852081,-31.2603591255822,-0.180655744950565));
#6986=CARTESIAN_POINT('Ctrl Pts',(9.25427310233174,-31.2847172168174,-0.111261144643989));
#6987=CARTESIAN_POINT('Ctrl Pts',(9.26514366379684,-31.3075704215151,-0.0418048433807318));
#6988=CARTESIAN_POINT('Ctrl Pts',(9.27825315802543,-31.3288352466054,0.0273873077103627));
#6989=CARTESIAN_POINT('Ctrl Pts',(9.28704721651805,-31.3431000315328,0.0738025098008598));
#6990=CARTESIAN_POINT('Ctrl Pts',(9.29684788658827,-31.3566506839595,0.120098937659176));
#6991=CARTESIAN_POINT('Ctrl Pts',(9.30761891872914,-31.3694699518936,0.166181422977337));
#6992=CARTESIAN_POINT('Ctrl Pts',(9.32367525640488,-31.3885795870719,0.234876412977284));
#6993=CARTESIAN_POINT('Ctrl Pts',(9.34225287296387,-31.4066143205822,0.303705335324998));
#6994=CARTESIAN_POINT('Ctrl Pts',(9.36331943904692,-31.4234647439641,0.37234447007711));
#6995=CARTESIAN_POINT('Ctrl Pts',(9.38435814667911,-31.440292884327,0.440892836359643));
#6996=CARTESIAN_POINT('Ctrl Pts',(9.40787918918951,-31.4559396029575,0.509251242356834));
#6997=CARTESIAN_POINT('Ctrl Pts',(9.4338025321309,-31.4703157961373,0.577093346534773));
#6998=CARTESIAN_POINT('Ctrl Pts',(9.45972752251909,-31.4846929029344,0.644939762126485));
#6999=CARTESIAN_POINT('Ctrl Pts',(9.48805494275305,-31.4977991390296,0.712269124557971));
#7000=CARTESIAN_POINT('Ctrl Pts',(9.51865844890992,-31.5095684826672,0.778761359262283));
#7001=CARTESIAN_POINT('Ctrl Pts',(9.54925455115649,-31.5213349789459,0.84523750749142));
#7002=CARTESIAN_POINT('Ctrl Pts',(9.58212531838652,-31.5317651226119,0.910876280137526));
#7003=CARTESIAN_POINT('Ctrl Pts',(9.61710196385504,-31.5408182147074,0.975374241033881));
#7004=CARTESIAN_POINT('Ctrl Pts',(9.6521317708761,-31.5498850667397,1.03997023339355));
#7005=CARTESIAN_POINT('Ctrl Pts',(9.6892734311385,-31.557570645475,1.10342135481135));
#7006=CARTESIAN_POINT('Ctrl Pts',(9.7283203630777,-31.563860483921,1.16544861040227));
#7007=CARTESIAN_POINT('Ctrl Pts',(9.75451366980933,-31.5680798081937,1.20705748594579));
#7008=CARTESIAN_POINT('Ctrl Pts',(9.78156357052936,-31.5716716126613,1.24802618569463));
#7009=CARTESIAN_POINT('Ctrl Pts',(9.80940000840292,-31.5746381640016,1.28827884419634));
#7010=CARTESIAN_POINT('Ctrl Pts',(9.85089568312997,-31.5790603910853,1.34828333297731));
#7011=CARTESIAN_POINT('Ctrl Pts',(9.89472960492287,-31.5825133899701,1.40722791797293));
#7012=CARTESIAN_POINT('Ctrl Pts',(9.94074551483348,-31.584959302977,1.46480935021338));
#7013=CARTESIAN_POINT('Ctrl Pts',(9.98670057325285,-31.5874019815058,1.52231463670281));
#7014=CARTESIAN_POINT('Ctrl Pts',(10.0348315554065,-31.5888401448587,1.57845972694491));
#7015=CARTESIAN_POINT('Ctrl Pts',(10.0849379261036,-31.5892542604541,1.63296134034101));
#7016=CARTESIAN_POINT('Ctrl Pts',(10.1350474810957,-31.5896684023668,1.68746641735299));
#7017=CARTESIAN_POINT('Ctrl Pts',(10.1871322473094,-31.5890583283654,1.74032721705655));
#7018=CARTESIAN_POINT('Ctrl Pts',(10.2409521642725,-31.5874236709743,1.79128851362573));
#7019=CARTESIAN_POINT('Ctrl Pts',(10.294759060576,-31.5857894090561,1.84223748112165));
#7020=CARTESIAN_POINT('Ctrl Pts',(10.350299722244,-31.5831310830658,1.89128737321192));
#7021=CARTESIAN_POINT('Ctrl Pts',(10.4073021361898,-31.5794675918019,1.93821939640097));
#7022=CARTESIAN_POINT('Ctrl Pts',(10.4643911889991,-31.5757985323401,1.98522275230865));
#7023=CARTESIAN_POINT('Ctrl Pts',(10.5229458190115,-31.5711213272259,2.03010142110689));
#7024=CARTESIAN_POINT('Ctrl Pts',(10.5826693342582,-31.5654735347332,2.07267852251315));
#7025=CARTESIAN_POINT('Ctrl Pts',(10.6227328239173,-31.5616849051592,2.10123992340947));
#7026=CARTESIAN_POINT('Ctrl Pts',(10.663321827487,-31.5574599049519,2.12876654161601));
#7027=CARTESIAN_POINT('Ctrl Pts',(10.7043430819144,-31.5528141989058,2.15521684061908));
#7028=CARTESIAN_POINT('Ctrl Pts',(10.7654933137918,-31.5458888621279,2.19464620327128));
#7029=CARTESIAN_POINT('Ctrl Pts',(10.8283682976571,-31.5383484986996,2.23203175294854));
#7030=CARTESIAN_POINT('Ctrl Pts',(10.8927078099178,-31.5302152749572,2.26715077383221));
#7031=CARTESIAN_POINT('Ctrl Pts',(10.9569622395341,-31.5220928065992,2.30222335328266));
#7032=CARTESIAN_POINT('Ctrl Pts',(11.0226768047413,-31.5133790835425,2.33503490407232));
#7033=CARTESIAN_POINT('Ctrl Pts',(11.0895585832631,-31.5041079129142,2.36540131373456));
#7034=CARTESIAN_POINT('Ctrl Pts',(11.1564446121696,-31.4948361530965,2.39576965320377));
#7035=CARTESIAN_POINT('Ctrl Pts',(11.2244973822511,-31.4850069477636,2.42369216050305));
#7036=CARTESIAN_POINT('Ctrl Pts',(11.2933987451609,-31.4746650134954,2.44902900915238));
#7037=CARTESIAN_POINT('Ctrl Pts',(11.362283438755,-31.4643255812527,2.47435972805461));
#7038=CARTESIAN_POINT('Ctrl Pts',(11.4320156256799,-31.4534737743353,2.49710580690326));
#7039=CARTESIAN_POINT('Ctrl Pts',(11.5022620939793,-31.4421638247251,2.51717642960905));
#7040=CARTESIAN_POINT('Ctrl Pts',(11.5726153309883,-31.4308366849451,2.53727755796928));
#7041=CARTESIAN_POINT('Ctrl Pts',(11.6434837004321,-31.4190501390555,2.55469500339208));
#7042=CARTESIAN_POINT('Ctrl Pts',(11.7145276936783,-31.4068664655425,2.56938903350662));
#7043=CARTESIAN_POINT('Ctrl Pts',(11.7621851411177,-31.3986934623999,2.57924602402558));
#7044=CARTESIAN_POINT('Ctrl Pts',(11.8099215343715,-31.3903419148347,2.58787857636211));
#7045=CARTESIAN_POINT('Ctrl Pts',(11.8576356015541,-31.3818321115427,2.59528770975726));
#7046=CARTESIAN_POINT('Ctrl Pts',(11.92876278459,-31.3691465793279,2.60633247743796));
#7047=CARTESIAN_POINT('Ctrl Pts',(12.0006922714993,-31.3563785961297,2.61475432517957));
#7048=CARTESIAN_POINT('Ctrl Pts',(12.0731004304628,-31.3435869370415,2.62045518191386));
#7049=CARTESIAN_POINT('Ctrl Pts',(12.1454128367948,-31.3308121936578,2.62614849982874));
#7050=CARTESIAN_POINT('Ctrl Pts',(12.218201984195,-31.3180139586677,2.62912778112531));
#7051=CARTESIAN_POINT('Ctrl Pts',(12.2911289753557,-31.3052525828952,2.62934454720093));
#7052=CARTESIAN_POINT('Ctrl Pts',(12.3640606010783,-31.2924903961283,2.6295613270522));
#7053=CARTESIAN_POINT('Ctrl Pts',(12.4371293739151,-31.2797652002543,2.62701514692943));
#7054=CARTESIAN_POINT('Ctrl Pts',(12.5099901525806,-31.2671372962338,2.62170927404779));
#7055=CARTESIAN_POINT('Ctrl Pts',(12.5828333040285,-31.2545124472838,2.61640468481667));
#7056=CARTESIAN_POINT('Ctrl Pts',(12.655467841404,-31.2419849675523,2.60834181054521));
#7057=CARTESIAN_POINT('Ctrl Pts',(12.727553502541,-31.2296131594624,2.59757579979063));
#7058=CARTESIAN_POINT('Ctrl Pts',(12.7997487278055,-31.2172225472672,2.58679342560739));
#7059=CARTESIAN_POINT('Ctrl Pts',(12.8713927192491,-31.2049881958071,2.57329990897772));
#7060=CARTESIAN_POINT('Ctrl Pts',(12.9421589256818,-31.1929649025856,2.55720053492581));
#7061=CARTESIAN_POINT('Ctrl Pts',(12.9896300292815,-31.1848994851089,2.54640081720695));
#7062=CARTESIAN_POINT('Ctrl Pts',(13.0367064708688,-31.1769289608158,2.53442952081183));
#7063=CARTESIAN_POINT('Ctrl Pts',(13.0832957533592,-31.1690685522685,2.52133001886305));
#7064=CARTESIAN_POINT('Ctrl Pts',(13.152746224025,-31.1573510703918,2.50180263987797));
#7065=CARTESIAN_POINT('Ctrl Pts',(13.2219502995756,-31.1461566041751,2.4795927354516));
#7066=CARTESIAN_POINT('Ctrl Pts',(13.2905740551594,-31.1355498713967,2.454746303444));
#7067=CARTESIAN_POINT('Ctrl Pts',(13.3591070626113,-31.1249571649737,2.42993272838613));
#7068=CARTESIAN_POINT('Ctrl Pts',(13.4270605835757,-31.1149507802081,2.40248965699016));
#7069=CARTESIAN_POINT('Ctrl Pts',(13.4941052636855,-31.1055855583044,2.37251384629929));
#7070=CARTESIAN_POINT('Ctrl Pts',(13.561154204532,-31.0962197412342,2.3425361306245));
#7071=CARTESIAN_POINT('Ctrl Pts',(13.6272934981485,-31.0874952820534,2.31002556527993));
#7072=CARTESIAN_POINT('Ctrl Pts',(13.6922074515289,-31.0794554797504,2.27512786406386));
#7073=CARTESIAN_POINT('Ctrl Pts',(13.7571057002679,-31.0714176225178,2.2402386056533));
#7074=CARTESIAN_POINT('Ctrl Pts',(13.820778567186,-31.0640641656373,2.20296372939604));
#7075=CARTESIAN_POINT('Ctrl Pts',(13.8829342849464,-31.0574254130287,2.16349342564774));
#7076=CARTESIAN_POINT('Ctrl Pts',(13.9451844741581,-31.0507765700758,2.12396313036507));
#7077=CARTESIAN_POINT('Ctrl Pts',(14.0059123487213,-31.0448446416354,2.08223120813844));
#7078=CARTESIAN_POINT('Ctrl Pts',(14.0648575226134,-31.0396462247334,2.03852710839681));
#7079=CARTESIAN_POINT('Ctrl Pts',(14.1043988884374,-31.0361590434961,2.00920969898413));
#7080=CARTESIAN_POINT('Ctrl Pts',(14.1431387485305,-31.033001646773,1.97900561592663));
#7081=CARTESIAN_POINT('Ctrl Pts',(14.1810084262852,-31.0301755043672,1.94799199564959));
#7082=CARTESIAN_POINT('Ctrl Pts',(14.2374606145018,-31.0259625843616,1.90176010689422));
#7083=CARTESIAN_POINT('Ctrl Pts',(14.2926991654363,-31.0228311175415,1.85331739425799));
#7084=CARTESIAN_POINT('Ctrl Pts',(14.3464350150607,-31.0208199212765,1.80284481408892));
#7085=CARTESIAN_POINT('Ctrl Pts',(14.4000998043365,-31.0188113846198,1.75243897891727));
#7086=CARTESIAN_POINT('Ctrl Pts',(14.4522652453566,-31.0179202520598,1.70000899168618));
#7087=CARTESIAN_POINT('Ctrl Pts',(14.502665154571,-31.0181648931129,1.64577768116561));
#7088=CARTESIAN_POINT('Ctrl Pts',(14.5530682667356,-31.0184095497132,1.59154292420659));
#7089=CARTESIAN_POINT('Ctrl Pts',(14.6017050675006,-31.0197901594918,1.53550708982247));
#7090=CARTESIAN_POINT('Ctrl Pts',(14.6483399207647,-31.0223038005615,1.47792947798989));
#7091=CARTESIAN_POINT('Ctrl Pts',(14.6949634916526,-31.0248168335058,1.42036579591648));
#7092=CARTESIAN_POINT('Ctrl Pts',(14.7395856359476,-31.02846231646,1.3612616640622));
#7093=CARTESIAN_POINT('Ctrl Pts',(14.7820090211866,-31.0332160313446,1.30090464504866));
#7094=CARTESIAN_POINT('Ctrl Pts',(14.8244968863946,-31.037976971475,1.24045588845464));
#7095=CARTESIAN_POINT('Ctrl Pts',(14.8647789760217,-31.0438494224712,1.17875107963657));
#7096=CARTESIAN_POINT('Ctrl Pts',(14.9027011721154,-31.0507886274603,1.11609838715478));
#7097=CARTESIAN_POINT('Ctrl Pts',(14.9281399880451,-31.0554435572006,1.07406995853712));
#7098=CARTESIAN_POINT('Ctrl Pts',(14.9525177990215,-31.0605780934011,1.03161537789579));
#7099=CARTESIAN_POINT('Ctrl Pts',(14.975800076653,-31.0661739903831,0.988830267143717));
#7100=CARTESIAN_POINT('Ctrl Pts',(15.0105068815928,-31.074515773266,0.925050661183067));
#7101=CARTESIAN_POINT('Ctrl Pts',(15.0433058380794,-31.0843398123408,0.85996981368557));
#7102=CARTESIAN_POINT('Ctrl Pts',(15.0739990115275,-31.0956323113691,0.793867798863216));
#7103=CARTESIAN_POINT('Ctrl Pts',(15.1046515962884,-31.1069098771839,0.727853197419949));
#7104=CARTESIAN_POINT('Ctrl Pts',(15.1332035267178,-31.1196520113202,0.660820696335817));
#7105=CARTESIAN_POINT('Ctrl Pts',(15.1594929062039,-31.1338168732025,0.593075062136874));
#7106=CARTESIAN_POINT('Ctrl Pts',(15.1857839563985,-31.1479826352717,0.525325122655191));
#7107=CARTESIAN_POINT('Ctrl Pts',(15.2098118340435,-31.1635712134381,0.456862603465919));
#7108=CARTESIAN_POINT('Ctrl Pts',(15.2314557123161,-31.1805134006464,0.388009033183554));
#7109=CARTESIAN_POINT('Ctrl Pts',(15.2530943542826,-31.1974514890293,0.319172120653958));
#7110=CARTESIAN_POINT('Ctrl Pts',(15.2723499530455,-31.2157423538751,0.249945031380815));
#7111=CARTESIAN_POINT('Ctrl Pts',(15.2891468470745,-31.2352915303582,0.180655744947757));
#7112=CARTESIAN_POINT('Ctrl Pts',(15.3059692709664,-31.2548704199413,0.111261144641073));
#7113=CARTESIAN_POINT('Ctrl Pts',(15.3203254460599,-31.2757112046725,0.0418048433777034));
#7114=CARTESIAN_POINT('Ctrl Pts',(15.3321865776807,-31.2976967722504,-0.0273873077134898));
#7115=CARTESIAN_POINT('Ctrl Pts',(15.3401432145609,-31.3124450427708,-0.0738025098029384));
#7116=CARTESIAN_POINT('Ctrl Pts',(15.346978088765,-31.3277079982387,-0.120098937660215));
#7117=CARTESIAN_POINT('Ctrl Pts',(15.3526943843833,-31.3434456196644,-0.166181422977341));
#7118=CARTESIAN_POINT('Ctrl Pts',(15.3612156450668,-31.3669056335723,-0.234876412976922));
#7119=CARTESIAN_POINT('Ctrl Pts',(15.3675453741577,-31.3920116882092,-0.303705335324268));
#7120=CARTESIAN_POINT('Ctrl Pts',(15.3716049858294,-31.4186810812984,-0.372344470076017));
#7121=CARTESIAN_POINT('Ctrl Pts',(15.3756592290661,-31.4453152067524,-0.440892836359328));
#7122=CARTESIAN_POINT('Ctrl Pts',(15.3774491636308,-31.4735083864055,-0.509251242357308));
#7123=CARTESIAN_POINT('Ctrl Pts',(15.3769376406635,-31.503146756534,-0.577093346536008));
#7124=CARTESIAN_POINT('Ctrl Pts',(15.3764260851886,-31.5327870102016,-0.644939762127695));
#7125=CARTESIAN_POINT('Ctrl Pts',(15.3736127084781,-31.5638723937955,-0.712269124559153));
#7126=CARTESIAN_POINT('Ctrl Pts',(15.3685035059756,-31.596260479391,-0.778761359263442));
#7127=CARTESIAN_POINT('Ctrl Pts',(15.3633955395432,-31.6286407293327,-0.845237507492574));
#7128=CARTESIAN_POINT('Ctrl Pts',(15.355992925308,-31.6623227206288,-0.910876280138652));
#7129=CARTESIAN_POINT('Ctrl Pts',(15.3463448103112,-31.6971399301915,-0.975374241034996));
#7130=CARTESIAN_POINT('Ctrl Pts',(15.336682030993,-31.7320100589774,-1.03997023339446));
#7131=CARTESIAN_POINT('Ctrl Pts',(15.3247671072894,-31.768018469671,-1.10342135481207));
#7132=CARTESIAN_POINT('Ctrl Pts',(15.3106908011997,-31.804979023893,-1.16544861040279));
#7133=CARTESIAN_POINT('Ctrl Pts',(15.301248189841,-31.829772755068,-1.20705748594613));
#7134=CARTESIAN_POINT('Ctrl Pts',(15.2908338333953,-31.8549945584951,-1.2480261856948));
#7135=CARTESIAN_POINT('Ctrl Pts',(15.2794847232809,-31.8805848965145,-1.28827884419633));
#7136=CARTESIAN_POINT('Ctrl Pts',(15.2625666469132,-31.9187323185172,-1.34828333297744));
#7137=CARTESIAN_POINT('Ctrl Pts',(15.2436400707701,-31.9584201077799,-1.40722791797319));
#7138=CARTESIAN_POINT('Ctrl Pts',(15.2227503386142,-31.9994940112443,-1.46480935021377));
#7139=CARTESIAN_POINT('Ctrl Pts',(15.201888231064,-32.0405135985318,-1.5223146367026));
#7140=CARTESIAN_POINT('Ctrl Pts',(15.1790682259857,-32.082915333462,-1.57845972694411));
#7141=CARTESIAN_POINT('Ctrl Pts',(15.1543736752632,-32.1265157811743,-1.63296134033967));
#7142=CARTESIAN_POINT('Ctrl Pts',(15.1296775551844,-32.1701189997261,-1.68746641735158));
#7143=CARTESIAN_POINT('Ctrl Pts',(15.1031068324942,-32.2149206934165,-1.74032721705509));
#7144=CARTESIAN_POINT('Ctrl Pts',(15.0747812191856,-32.2607127800405,-1.79128851362422));
#7145=CARTESIAN_POINT('Ctrl Pts',(15.0464624586962,-32.3064937881792,-1.84223748112036));
#7146=CARTESIAN_POINT('Ctrl Pts',(15.016389950023,-32.3532642491317,-1.89128737321084));
#7147=CARTESIAN_POINT('Ctrl Pts',(14.9847160665489,-32.4007980420539,-1.93821939640007));
#7148=CARTESIAN_POINT('Ctrl Pts',(14.9529940414421,-32.4484040823342,-1.98522275230807));
#7149=CARTESIAN_POINT('Ctrl Pts',(14.9196661479882,-32.4967752768773,-2.03010142110661));
#7150=CARTESIAN_POINT('Ctrl Pts',(14.8849132585906,-32.5456734620382,-2.07267852251313));
#7151=CARTESIAN_POINT('Ctrl Pts',(14.8616004643044,-32.5784751470602,-2.10123992340946));
#7152=CARTESIAN_POINT('Ctrl Pts',(14.8376470050091,-32.6115137551623,-2.12876654161601));
#7153=CARTESIAN_POINT('Ctrl Pts',(14.8131130783409,-32.6447163505684,-2.15521684061908));
#7154=CARTESIAN_POINT('Ctrl Pts',(14.7765404448228,-32.6942113364327,-2.1946462032713));
#7155=CARTESIAN_POINT('Ctrl Pts',(14.7385728066074,-32.7448924880085,-2.2320317529486));
#7156=CARTESIAN_POINT('Ctrl Pts',(14.6993594721015,-32.7965455282222,-2.2671507738323));
#7157=CARTESIAN_POINT('Ctrl Pts',(14.6601979933537,-32.8481302623967,-2.30222335328281));
#7158=CARTESIAN_POINT('Ctrl Pts',(14.6197944052214,-32.9006838837365,-2.33503490407254));
#7159=CARTESIAN_POINT('Ctrl Pts',(14.5783244466735,-32.9539696176727,-2.36540131373483));
#7160=CARTESIAN_POINT('Ctrl Pts',(14.5368518526803,-33.007258737955,-2.39576965320397));
#7161=CARTESIAN_POINT('Ctrl Pts',(14.4943131261224,-33.0612795629769,-2.42369216050319));
#7162=CARTESIAN_POINT('Ctrl Pts',(14.450906066867,-33.115778926478,-2.44902900915247));
#7163=CARTESIAN_POINT('Ctrl Pts',(14.4075095090871,-33.1702651049412,-2.47435972805472));
#7164=CARTESIAN_POINT('Ctrl Pts',(14.3632454751571,-33.2252290468209,-2.4971058069034));
#7165=CARTESIAN_POINT('Ctrl Pts',(14.3183275373294,-33.2804092980893,-2.5171764296092));
#7166=CARTESIAN_POINT('Ctrl Pts',(14.2733413280232,-33.3356734186875,-2.53727755796941));
#7167=CARTESIAN_POINT('Ctrl Pts',(14.2276996951381,-33.3911539540059,-2.5546950033922));
#7168=CARTESIAN_POINT('Ctrl Pts',(14.1816263277413,-33.4465880201868,-2.56938903350673));
#7169=CARTESIAN_POINT('Ctrl Pts',(14.150719575675,-33.4837740787775,-2.57924602402564));
#7170=CARTESIAN_POINT('Ctrl Pts',(14.1196187266958,-33.5209392342376,-2.58787857636214));
#7171=CARTESIAN_POINT('Ctrl Pts',(14.0883919872725,-33.5580059268895,-2.59528770975726));
#7172=CARTESIAN_POINT('Ctrl Pts',(14.0418424025961,-33.6132611081907,-2.60633247743793));
#7173=CARTESIAN_POINT('Ctrl Pts',(13.9948202613369,-33.6691698795361,-2.61475432517952));
#7174=CARTESIAN_POINT('Ctrl Pts',(13.9475382801283,-33.7254813550954,-2.62045518191382));
#7175=CARTESIAN_POINT('Ctrl Pts',(13.900318824665,-33.7817183642961,-2.62614849982874));
#7176=CARTESIAN_POINT('Ctrl Pts',(13.8528406543396,-33.8383564975698,-2.62912778112532));
#7177=CARTESIAN_POINT('Ctrl Pts',(13.8053254831527,-33.8951324366506,-2.62934454720094));
#7178=CARTESIAN_POINT('Ctrl Pts',(13.7578072923433,-33.9519119838823,-2.62956132705218));
#7179=CARTESIAN_POINT('Ctrl Pts',(13.7102525630299,-34.0088287994454,-2.6270151469294));
#7180=CARTESIAN_POINT('Ctrl Pts',(13.6628860880188,-34.065614132699,-2.62170927404773));
#7181=CARTESIAN_POINT('Ctrl Pts',(13.6155310723855,-34.1223857278693,-2.61640468481661));
#7182=CARTESIAN_POINT('Ctrl Pts',(13.5683646880051,-34.1790253425627,-2.60834181054517));
#7183=CARTESIAN_POINT('Ctrl Pts',(13.5216075573401,-34.2352674523107,-2.59757579979065));
#7184=CARTESIAN_POINT('Ctrl Pts',(13.4747793597782,-34.2915950453243,-2.58679342560735));
#7185=CARTESIAN_POINT('Ctrl Pts',(13.4283621048929,-34.3475233862133,-2.5732999089776));
#7186=CARTESIAN_POINT('Ctrl Pts',(13.3825665243094,-34.402797072103,-2.5572005349256));
#7187=CARTESIAN_POINT('Ctrl Pts',(13.3518461160827,-34.4398755450274,-2.54640081720679));
#7188=CARTESIAN_POINT('Ctrl Pts',(13.32140521877,-34.476659677215,-2.53442952081174));
#7189=CARTESIAN_POINT('Ctrl Pts',(13.291303264039,-34.5130769751218,-2.52133001886304));
#7190=CARTESIAN_POINT('Ctrl Pts',(13.2464303917327,-34.5673641060844,-2.50180263987811));
#7191=CARTESIAN_POINT('Ctrl Pts',(13.2021336618323,-34.6216993604479,-2.47959273545193));
#7192=CARTESIAN_POINT('Ctrl Pts',(13.1586360840035,-34.675825909697,-2.45474630344456));
#7193=CARTESIAN_POINT('Ctrl Pts',(13.1151960274206,-34.7298808819363,-2.42993272838686));
#7194=CARTESIAN_POINT('Ctrl Pts',(13.0725534835316,-34.783727164985,-2.40248965699108));
#7195=CARTESIAN_POINT('Ctrl Pts',(13.0309206233962,-34.8371069501965,-2.37251384630043));
#7196=CARTESIAN_POINT('Ctrl Pts',(12.9892851174628,-34.8904901277314,-2.34253613062566));
#7197=CARTESIAN_POINT('Ctrl Pts',(12.9486598673696,-34.9434062066014,-2.31002556528109));
#7198=CARTESIAN_POINT('Ctrl Pts',(12.9092402176435,-34.9956034381375,-2.27512786406503));
#7199=CARTESIAN_POINT('Ctrl Pts',(12.869830104718,-35.0477880415911,-2.24023860565402));
#7200=CARTESIAN_POINT('Ctrl Pts',(12.8316253907942,-35.0992536334345,-2.20296372939623));
#7201=CARTESIAN_POINT('Ctrl Pts',(12.794798203505,-35.1497626877019,-2.16349342564734));
#7202=CARTESIAN_POINT('Ctrl Pts',(12.7579150419963,-35.200348511473,-2.12396313036471));
#7203=CARTESIAN_POINT('Ctrl Pts',(12.7224139039918,-35.2499744293424,-2.0822312081381));
#7204=CARTESIAN_POINT('Ctrl Pts',(12.6884393559493,-35.2984232389124,-2.0385271083965));
#7205=CARTESIAN_POINT('Ctrl Pts',(12.6656486854982,-35.3309234755976,-2.00920969898392));
#7206=CARTESIAN_POINT('Ctrl Pts',(12.6435443696797,-35.3628944802155,-1.97900561592653));
#7207=CARTESIAN_POINT('Ctrl Pts',(12.6221620196843,-35.3942775119812,-1.94799199564959));
#7208=CARTESIAN_POINT('Ctrl Pts',(12.5902874298269,-35.4410600810735,-1.90176010689391));
#7209=CARTESIAN_POINT('Ctrl Pts',(12.559956224542,-35.4873323360413,-1.85331739425731));
#7210=CARTESIAN_POINT('Ctrl Pts',(12.5313465526722,-35.5328633487778,-1.80284481408786));
#7211=CARTESIAN_POINT('Ctrl Pts',(12.5027747142649,-35.5783341512515,-1.7524389789157));
#7212=CARTESIAN_POINT('Ctrl Pts',(12.4759202503196,-35.6230651820949,-1.70000899168406));
#7213=CARTESIAN_POINT('Ctrl Pts',(12.450932161079,-35.66683510435,-1.64577768116292));
#7214=CARTESIAN_POINT('Ctrl Pts',(12.4259424838277,-35.7106078082145,-1.59154292420375));
#7215=CARTESIAN_POINT('Ctrl Pts',(12.4028197265862,-35.7534188181251,-1.53550708981947));
#7216=CARTESIAN_POINT('Ctrl Pts',(12.3816791769766,-35.7950626062884,-1.47792947798673));
#7217=CARTESIAN_POINT('Ctrl Pts',(12.3605437419031,-35.8366963195644,-1.42036579591363));
#7218=CARTESIAN_POINT('Ctrl Pts',(12.3413897506033,-35.877162971572,-1.3612616640597));
#7219=CARTESIAN_POINT('Ctrl Pts',(12.3242948958363,-35.9162795583455,-1.30090464504652));
#7220=CARTESIAN_POINT('Ctrl Pts',(12.3071740583312,-35.9554555990333,-1.24045588845259));
#7221=CARTESIAN_POINT('Ctrl Pts',(12.2921187052629,-35.9932771374658,-1.17875107963462));
#7222=CARTESIAN_POINT('Ctrl Pts',(12.2791671350188,-36.0295883251447,-1.11609838715294));
#7223=CARTESIAN_POINT('Ctrl Pts',(12.270479014462,-36.0539464508519,-1.07406995853587));
#7224=CARTESIAN_POINT('Ctrl Pts',(12.2627367477602,-36.0776255225459,-1.03161537789517));
#7225=CARTESIAN_POINT('Ctrl Pts',(12.255941797888,-36.1005865149234,-0.988830267143708));
#7226=CARTESIAN_POINT('Ctrl Pts',(12.2458125913075,-36.1348143811267,-0.925050661183478));
#7227=CARTESIAN_POINT('Ctrl Pts',(12.2379209804709,-36.1681311301989,-0.859969813686402));
#7228=CARTESIAN_POINT('Ctrl Pts',(12.2323539847775,-36.2003584476417,-0.793867798864489));
#7229=CARTESIAN_POINT('Ctrl Pts',(12.2267943508855,-36.2325431476436,-0.727853197421361));
#7230=CARTESIAN_POINT('Ctrl Pts',(12.2235533975312,-36.2636409117907,-0.660820696337379));
#7231=CARTESIAN_POINT('Ctrl Pts',(12.2226758380193,-36.2934906132165,-0.593075062138574));
#7232=CARTESIAN_POINT('Ctrl Pts',(12.2217982227379,-36.3233422116119,-0.52532512265681));
#7233=CARTESIAN_POINT('Ctrl Pts',(12.2232843886163,-36.3519452531347,-0.456862603467453));
#7234=CARTESIAN_POINT('Ctrl Pts',(12.2271348139981,-36.3791604951594,-0.388009033184998));
#7235=CARTESIAN_POINT('Ctrl Pts',(12.2309843078459,-36.406369152997,-0.319172120656019));
#7236=CARTESIAN_POINT('Ctrl Pts',(12.237196862078,-36.4321904231135,-0.249945031383509));
#7237=CARTESIAN_POINT('Ctrl Pts',(12.2457284985207,-36.4565115482887,-0.18065574495107));
#7238=CARTESIAN_POINT('Ctrl Pts',(12.2542731023316,-36.4808696395237,-0.111261144644779));
#7239=CARTESIAN_POINT('Ctrl Pts',(12.2651436637966,-36.5037228442214,-0.0418048433818011));
#7240=CARTESIAN_POINT('Ctrl Pts',(12.2782531580251,-36.5249876693116,0.0273873077090091));
#7241=CARTESIAN_POINT('Ctrl Pts',(12.2870472165178,-36.5392524542392,0.0738025097999603));
#7242=CARTESIAN_POINT('Ctrl Pts',(12.2968478865881,-36.552803106666,0.120098937658729));
#7243=CARTESIAN_POINT('Ctrl Pts',(12.3076189187291,-36.5656223746002,0.16618142297734));
#7244=CARTESIAN_POINT('Ctrl Pts',(12.3236752564048,-36.5847320097785,0.23487641297725));
#7245=CARTESIAN_POINT('Ctrl Pts',(12.3422528729638,-36.6027667432888,0.303705335324935));
#7246=CARTESIAN_POINT('Ctrl Pts',(12.3633194390469,-36.6196171666707,0.372344470077012));
#7247=CARTESIAN_POINT('Ctrl Pts',(12.3843581466792,-36.6364453070337,0.440892836359892));
#7248=CARTESIAN_POINT('Ctrl Pts',(12.4078791891897,-36.6520920256643,0.50925124235744));
#7249=CARTESIAN_POINT('Ctrl Pts',(12.4338025321312,-36.6664682188442,0.577093346535715));
#7250=CARTESIAN_POINT('Ctrl Pts',(12.4597275225194,-36.6808453256412,0.644939762127416));
#7251=CARTESIAN_POINT('Ctrl Pts',(12.4880549427534,-36.6939515617364,0.712269124558878));
#7252=CARTESIAN_POINT('Ctrl Pts',(12.5186584489103,-36.705720905374,0.77876135926318));
#7253=CARTESIAN_POINT('Ctrl Pts',(12.5492545511566,-36.7174874016526,0.845237507491614));
#7254=CARTESIAN_POINT('Ctrl Pts',(12.5821253183863,-36.7279175453184,0.910876280137029));
#7255=CARTESIAN_POINT('Ctrl Pts',(12.6171019638544,-36.7369706374139,0.975374241032723));
#7256=CARTESIAN_POINT('Ctrl Pts',(12.6521317708754,-36.7460374894462,1.03997023339245));
#7257=CARTESIAN_POINT('Ctrl Pts',(12.6892734311378,-36.7537230681815,1.10342135481031));
#7258=CARTESIAN_POINT('Ctrl Pts',(12.7283203630771,-36.7600129066275,1.16544861040129));
#7259=CARTESIAN_POINT('Ctrl Pts',(12.7545136698089,-36.7642322309003,1.20705748594514));
#7260=CARTESIAN_POINT('Ctrl Pts',(12.7815635705291,-36.7678240353679,1.24802618569432));
#7261=CARTESIAN_POINT('Ctrl Pts',(12.8094000084029,-36.7707905867082,1.28827884419634));
#7262=CARTESIAN_POINT('Ctrl Pts',(12.8508956831299,-36.775212813792,1.34828333297722));
#7263=CARTESIAN_POINT('Ctrl Pts',(12.8947296049227,-36.7786658126767,1.40722791797275));
#7264=CARTESIAN_POINT('Ctrl Pts',(12.9407455148333,-36.7811117256837,1.46480935021313));
#7265=CARTESIAN_POINT('Ctrl Pts',(12.9867005732529,-36.7835544042125,1.52231463670294));
#7266=CARTESIAN_POINT('Ctrl Pts',(13.0348315554069,-36.7849925675654,1.57845972694538));
#7267=CARTESIAN_POINT('Ctrl Pts',(13.0849379261043,-36.7854066831607,1.63296134034182));
#7268=CARTESIAN_POINT('Ctrl Pts',(13.1350474810965,-36.7858208250734,1.68746641735378));
#7269=CARTESIAN_POINT('Ctrl Pts',(13.1871322473101,-36.785210751072,1.74032721705733));
#7270=CARTESIAN_POINT('Ctrl Pts',(13.2409521642733,-36.7835760936809,1.79128851362649));
#7271=CARTESIAN_POINT('Ctrl Pts',(13.2947590605769,-36.7819418317627,1.84223748112254));
#7272=CARTESIAN_POINT('Ctrl Pts',(13.3502997222452,-36.7792835057724,1.89128737321292));
#7273=CARTESIAN_POINT('Ctrl Pts',(13.4073021361911,-36.7756200145084,1.93821939640206));
#7274=CARTESIAN_POINT('Ctrl Pts',(13.4643911890004,-36.7719509550466,1.98522275230973));
#7275=CARTESIAN_POINT('Ctrl Pts',(13.5229458190128,-36.7672737499325,2.03010142110795));
#7276=CARTESIAN_POINT('Ctrl Pts',(13.5826693342596,-36.7616259574397,2.07267852251418));
#7277=CARTESIAN_POINT('Ctrl Pts',(13.6227328239182,-36.7578373278657,2.10123992341013));
#7278=CARTESIAN_POINT('Ctrl Pts',(13.6633218274875,-36.7536123276585,2.12876654161633));
#7279=CARTESIAN_POINT('Ctrl Pts',(13.7043430819143,-36.7489666216124,2.15521684061907));
#7280=CARTESIAN_POINT('Ctrl Pts',(13.7654933137917,-36.7420412848346,2.19464620327122));
#7281=CARTESIAN_POINT('Ctrl Pts',(13.8283682976569,-36.7345009214063,2.23203175294843));
#7282=CARTESIAN_POINT('Ctrl Pts',(13.8927078099174,-36.7263676976639,2.26715077383206));
#7283=CARTESIAN_POINT('Ctrl Pts',(13.9569622395338,-36.7182452293059,2.30222335328249));
#7284=CARTESIAN_POINT('Ctrl Pts',(14.0226768047409,-36.7095315062492,2.33503490407216));
#7285=CARTESIAN_POINT('Ctrl Pts',(14.0895585832627,-36.7002603356209,2.36540131373439));
#7286=CARTESIAN_POINT('Ctrl Pts',(14.1564446121692,-36.6909885758032,2.39576965320358));
#7287=CARTESIAN_POINT('Ctrl Pts',(14.2244973822506,-36.6811593704703,2.42369216050285));
#7288=CARTESIAN_POINT('Ctrl Pts',(14.2933987451604,-36.6708174362021,2.44902900915218));
#7289=CARTESIAN_POINT('Ctrl Pts',(14.3622834387544,-36.6604780039595,2.47435972805441));
#7290=CARTESIAN_POINT('Ctrl Pts',(14.4320156256792,-36.649626197042,2.49710580690308));
#7291=CARTESIAN_POINT('Ctrl Pts',(14.5022620939786,-36.6383162474319,2.51717642960887));
#7292=CARTESIAN_POINT('Ctrl Pts',(14.5726153309875,-36.6269891076519,2.53727755796908));
#7293=CARTESIAN_POINT('Ctrl Pts',(14.6434837004311,-36.6152025617624,2.55469500339187));
#7294=CARTESIAN_POINT('Ctrl Pts',(14.7145276936772,-36.6030188882494,2.5693890335064));
#7295=CARTESIAN_POINT('Ctrl Pts',(14.762185141117,-36.5948458851067,2.57924602402545));
#7296=CARTESIAN_POINT('Ctrl Pts',(14.8099215343711,-36.5864943375414,2.58787857636205));
#7297=CARTESIAN_POINT('Ctrl Pts',(14.8576356015541,-36.5779845342494,2.59528770975725));
#7298=CARTESIAN_POINT('Ctrl Pts',(14.9287627845898,-36.5652990020346,2.60633247743792));
#7299=CARTESIAN_POINT('Ctrl Pts',(15.0006922714988,-36.5525310188365,2.6147543251795));
#7300=CARTESIAN_POINT('Ctrl Pts',(15.0731004304621,-36.5397393597483,2.62045518191379));
#7301=CARTESIAN_POINT('Ctrl Pts',(15.145412836794,-36.5269646163646,2.6261484998287));
#7302=CARTESIAN_POINT('Ctrl Pts',(15.2182019841943,-36.5141663813745,2.62912778112528));
#7303=CARTESIAN_POINT('Ctrl Pts',(15.291128975355,-36.501405005602,2.62934454720092));
#7304=CARTESIAN_POINT('Ctrl Pts',(15.3640606010775,-36.488642818835,2.62956132705221));
#7305=CARTESIAN_POINT('Ctrl Pts',(15.4371293739142,-36.4759176229611,2.62701514692947));
#7306=CARTESIAN_POINT('Ctrl Pts',(15.5099901525795,-36.4632897189407,2.62170927404787));
#7307=CARTESIAN_POINT('Ctrl Pts',(15.5828333040276,-36.4506648699906,2.61640468481675));
#7308=CARTESIAN_POINT('Ctrl Pts',(15.6554678414036,-36.4381373902591,2.60834181054526));
#7309=CARTESIAN_POINT('Ctrl Pts',(15.7275535025409,-36.425765582169,2.59757579979065));
#7310=CARTESIAN_POINT('Ctrl Pts',(15.7997487278054,-36.4133749699738,2.58679342560739));
#7311=CARTESIAN_POINT('Ctrl Pts',(15.8713927192492,-36.4011406185138,2.57329990897769));
#7312=CARTESIAN_POINT('Ctrl Pts',(15.9421589256821,-36.3891173252922,2.55720053492575));
#7313=CARTESIAN_POINT('Ctrl Pts',(15.9896300292816,-36.3810519078155,2.54640081720691));
#7314=CARTESIAN_POINT('Ctrl Pts',(16.0367064708689,-36.3730813835224,2.53442952081181));
#7315=CARTESIAN_POINT('Ctrl Pts',(16.0832957533591,-36.3652209749752,2.52133001886304));
#7316=CARTESIAN_POINT('Ctrl Pts',(16.1527462240253,-36.3535034930984,2.50180263987787));
#7317=CARTESIAN_POINT('Ctrl Pts',(16.2219502995763,-36.3423090268816,2.47959273545136));
#7318=CARTESIAN_POINT('Ctrl Pts',(16.2905740551604,-36.3317022941032,2.4547463034436));
#7319=CARTESIAN_POINT('Ctrl Pts',(16.3591070626129,-36.3211095876801,2.42993272838552));
#7320=CARTESIAN_POINT('Ctrl Pts',(16.4270605835777,-36.3111032029145,2.40248965698929));
#7321=CARTESIAN_POINT('Ctrl Pts',(16.494105263688,-36.3017379810107,2.37251384629813));
#7322=CARTESIAN_POINT('Ctrl Pts',(16.5611542045347,-36.2923721639404,2.34253613062317));
#7323=CARTESIAN_POINT('Ctrl Pts',(16.6272934981514,-36.2836477047596,2.31002556527841));
#7324=CARTESIAN_POINT('Ctrl Pts',(16.692207451532,-36.2756079024566,2.27512786406214));
#7325=CARTESIAN_POINT('Ctrl Pts',(16.7571057002714,-36.267570045224,2.24023860565128));
#7326=CARTESIAN_POINT('Ctrl Pts',(16.8207785671899,-36.2602165883435,2.2029637293937));
#7327=CARTESIAN_POINT('Ctrl Pts',(16.8829342849506,-36.2535778357349,2.16349342564505));
#7328=CARTESIAN_POINT('Ctrl Pts',(16.9451844741622,-36.2469289927821,2.12396313036229));
#7329=CARTESIAN_POINT('Ctrl Pts',(17.0059123487253,-36.2409970643416,2.08223120813556));
#7330=CARTESIAN_POINT('Ctrl Pts',(17.0648575226173,-36.2357986474397,2.03852710839383));
#7331=CARTESIAN_POINT('Ctrl Pts',(17.10439888844,-36.2323114662026,2.00920969898208));
#7332=CARTESIAN_POINT('Ctrl Pts',(17.1431387485318,-36.2291540694795,1.97900561592558));
#7333=CARTESIAN_POINT('Ctrl Pts',(17.1810084262852,-36.2263279270739,1.94799199564959));
#7334=CARTESIAN_POINT('Ctrl Pts',(17.2374606145019,-36.2221150070683,1.90176010689407));
#7335=CARTESIAN_POINT('Ctrl Pts',(17.2926991654366,-36.2189835402481,1.85331739425768));
#7336=CARTESIAN_POINT('Ctrl Pts',(17.3464350150612,-36.2169723439831,1.80284481408843));
#7337=CARTESIAN_POINT('Ctrl Pts',(17.4000998043377,-36.2149638073264,1.75243897891608));
#7338=CARTESIAN_POINT('Ctrl Pts',(17.4522652453585,-36.2140726747664,1.70000899168421));
#7339=CARTESIAN_POINT('Ctrl Pts',(17.5026651545736,-36.2143173158196,1.64577768116285));
#7340=CARTESIAN_POINT('Ctrl Pts',(17.553068266738,-36.2145619724199,1.59154292420388));
#7341=CARTESIAN_POINT('Ctrl Pts',(17.6017050675028,-36.2159425821985,1.53550708981983));
#7342=CARTESIAN_POINT('Ctrl Pts',(17.6483399207667,-36.2184562232683,1.47792947798732));
#7343=CARTESIAN_POINT('Ctrl Pts',(17.6949634916545,-36.2209692562126,1.42036579591399));
#7344=CARTESIAN_POINT('Ctrl Pts',(17.7395856359494,-36.2246147391669,1.36126166405979));
#7345=CARTESIAN_POINT('Ctrl Pts',(17.7820090211882,-36.2293684540514,1.30090464504635));
#7346=CARTESIAN_POINT('Ctrl Pts',(17.824496886396,-36.2341293941818,1.24045588845241));
#7347=CARTESIAN_POINT('Ctrl Pts',(17.864778976023,-36.240001845178,1.17875107963445));
#7348=CARTESIAN_POINT('Ctrl Pts',(17.9027011721166,-36.2469410501671,1.11609838715275));
#7349=CARTESIAN_POINT('Ctrl Pts',(17.9281399880459,-36.2515959799074,1.07406995853575));
#7350=CARTESIAN_POINT('Ctrl Pts',(17.9525177990218,-36.2567305161078,1.0316153778951));
#7351=CARTESIAN_POINT('Ctrl Pts',(17.9758000766529,-36.2623264130898,0.988830267143709));
#7352=CARTESIAN_POINT('Ctrl Pts',(18.0105068815927,-36.2706681959726,0.925050661183277));
#7353=CARTESIAN_POINT('Ctrl Pts',(18.0433058380791,-36.2804922350474,0.859969813686007));
#7354=CARTESIAN_POINT('Ctrl Pts',(18.0739990115272,-36.2917847340756,0.793867798863887));
#7355=CARTESIAN_POINT('Ctrl Pts',(18.1046515962876,-36.3030622998902,0.727853197421574));
#7356=CARTESIAN_POINT('Ctrl Pts',(18.1332035267167,-36.3158044340263,0.660820696338441));
#7357=CARTESIAN_POINT('Ctrl Pts',(18.1594929062024,-36.3299692959084,0.593075062140492));
#7358=CARTESIAN_POINT('Ctrl Pts',(18.1857839563971,-36.3441350579776,0.5253251226589));
#7359=CARTESIAN_POINT('Ctrl Pts',(18.2098118340421,-36.3597236361438,0.456862603469714));
#7360=CARTESIAN_POINT('Ctrl Pts',(18.2314557123148,-36.3766658233521,0.38800903318743));
#7361=CARTESIAN_POINT('Ctrl Pts',(18.2530943542811,-36.3936039117347,0.319172120658737));
#7362=CARTESIAN_POINT('Ctrl Pts',(18.2723499530439,-36.4118947765802,0.249945031386501));
#7363=CARTESIAN_POINT('Ctrl Pts',(18.2891468470729,-36.431443953063,0.180655744954341));
#7364=CARTESIAN_POINT('Ctrl Pts',(18.3059692709647,-36.4510228426459,0.111261144648359));
#7365=CARTESIAN_POINT('Ctrl Pts',(18.3203254460583,-36.4718636273767,0.0418048433856814));
#7366=CARTESIAN_POINT('Ctrl Pts',(18.3321865776792,-36.4938491949543,-0.027387307704834));
#7367=CARTESIAN_POINT('Ctrl Pts',(18.34014321456,-36.5085974654755,-0.0738025097971843));
#7368=CARTESIAN_POINT('Ctrl Pts',(18.3469780887646,-36.5238604209444,-0.12009893765735));
#7369=CARTESIAN_POINT('Ctrl Pts',(18.3526943843832,-36.539598042371,-0.166181422977344));
#7370=CARTESIAN_POINT('Ctrl Pts',(18.3612156450669,-36.5630580562793,-0.234876412977713));
#7371=CARTESIAN_POINT('Ctrl Pts',(18.3675453741578,-36.5881641109164,-0.303705335325853));
#7372=CARTESIAN_POINT('Ctrl Pts',(18.3716049858295,-36.614833504006,-0.372344470078386));
#7373=CARTESIAN_POINT('Ctrl Pts',(18.3756592290661,-36.6414676294599,-0.440892836361369));
#7374=CARTESIAN_POINT('Ctrl Pts',(18.3774491636308,-36.6696608091128,-0.509251242359004));
#7375=CARTESIAN_POINT('Ctrl Pts',(18.3769376406635,-36.6992991792413,-0.577093346537381));
#7376=CARTESIAN_POINT('Ctrl Pts',(18.3764260851885,-36.728939432909,-0.644939762129239));
#7377=CARTESIAN_POINT('Ctrl Pts',(18.3736127084779,-36.7600248165029,-0.712269124560869));
#7378=CARTESIAN_POINT('Ctrl Pts',(18.3685035059754,-36.7924129020986,-0.778761359265312));
#7379=CARTESIAN_POINT('Ctrl Pts',(18.3633955395429,-36.8247931520403,-0.845237507494451));
#7380=CARTESIAN_POINT('Ctrl Pts',(18.3559929253077,-36.8584751433364,-0.910876280140545));
#7381=CARTESIAN_POINT('Ctrl Pts',(18.3463448103109,-36.8932923528991,-0.975374241036891));
#7382=CARTESIAN_POINT('Ctrl Pts',(18.3366820309926,-36.9281624816852,-1.03997023339647));
#7383=CARTESIAN_POINT('Ctrl Pts',(18.324767107289,-36.9641708923788,-1.10342135481419));
#7384=CARTESIAN_POINT('Ctrl Pts',(18.3106908011992,-37.001131446601,-1.16544861040502));
#7385=CARTESIAN_POINT('Ctrl Pts',(18.3012481898405,-37.0259251777756,-1.20705748594759));
#7386=CARTESIAN_POINT('Ctrl Pts',(18.2908338333951,-37.0511469812022,-1.24802618569552));
#7387=CARTESIAN_POINT('Ctrl Pts',(18.2794847232809,-37.0767373192211,-1.28827884419634));
#7388=CARTESIAN_POINT('Ctrl Pts',(18.2625666469133,-37.1148847412236,-1.34828333297701));
#7389=CARTESIAN_POINT('Ctrl Pts',(18.2436400707704,-37.154572530486,-1.40722791797235));
#7390=CARTESIAN_POINT('Ctrl Pts',(18.2227503386146,-37.1956464339501,-1.46480935021252));
#7391=CARTESIAN_POINT('Ctrl Pts',(18.2018882310642,-37.2366660212381,-1.52231463670205));
#7392=CARTESIAN_POINT('Ctrl Pts',(18.1790682259857,-37.2790677561687,-1.57845972694423));
#7393=CARTESIAN_POINT('Ctrl Pts',(18.1543736752628,-37.3226682038816,-1.63296134034042));
#7394=CARTESIAN_POINT('Ctrl Pts',(18.129677555184,-37.3662714224335,-1.68746641735244));
#7395=CARTESIAN_POINT('Ctrl Pts',(18.1031068324937,-37.411073116124,-1.74032721705606));
#7396=CARTESIAN_POINT('Ctrl Pts',(18.074781219185,-37.4568652027481,-1.79128851362529));
#7397=CARTESIAN_POINT('Ctrl Pts',(18.0464624586957,-37.5026462108866,-1.84223748112121));
#7398=CARTESIAN_POINT('Ctrl Pts',(18.0163899500225,-37.549416671839,-1.89128737321147));
#7399=CARTESIAN_POINT('Ctrl Pts',(17.9847160665486,-37.596950464761,-1.93821939640052));
#7400=CARTESIAN_POINT('Ctrl Pts',(17.952994041442,-37.644556505041,-1.98522275230822));
#7401=CARTESIAN_POINT('Ctrl Pts',(17.9196661479882,-37.6929276995838,-2.03010142110648));
#7402=CARTESIAN_POINT('Ctrl Pts',(17.8849132585909,-37.7418258847445,-2.07267852251276));
#7403=CARTESIAN_POINT('Ctrl Pts',(17.8616004643046,-37.7746275697666,-2.10123992340922));
#7404=CARTESIAN_POINT('Ctrl Pts',(17.8376470050092,-37.8076661778688,-2.12876654161589));
#7405=CARTESIAN_POINT('Ctrl Pts',(17.8131130783409,-37.8408687732751,-2.15521684061908));
#7406=CARTESIAN_POINT('Ctrl Pts',(17.7765404448226,-37.8903637591396,-2.19464620327149));
#7407=CARTESIAN_POINT('Ctrl Pts',(17.738572806607,-37.9410449107156,-2.23203175294895));
#7408=CARTESIAN_POINT('Ctrl Pts',(17.6993594721009,-37.9926979509295,-2.26715077383279));
#7409=CARTESIAN_POINT('Ctrl Pts',(17.660197993353,-38.0442826851043,-2.30222335328343));
#7410=CARTESIAN_POINT('Ctrl Pts',(17.6197944052205,-38.0968363064444,-2.33503490407327));
#7411=CARTESIAN_POINT('Ctrl Pts',(17.5783244466724,-38.1501220403808,-2.36540131373564));
#7412=CARTESIAN_POINT('Ctrl Pts',(17.536851852679,-38.2034111606634,-2.39576965320488));
#7413=CARTESIAN_POINT('Ctrl Pts',(17.4943131261208,-38.2574319856855,-2.42369216050416));
#7414=CARTESIAN_POINT('Ctrl Pts',(17.4509060668652,-38.3119313491869,-2.44902900915349));
#7415=CARTESIAN_POINT('Ctrl Pts',(17.4075095090855,-38.3664175276498,-2.47435972805555));
#7416=CARTESIAN_POINT('Ctrl Pts',(17.3632454751557,-38.4213814695292,-2.49710580690407));
#7417=CARTESIAN_POINT('Ctrl Pts',(17.3183275373282,-38.4765617207974,-2.51717642960973));
#7418=CARTESIAN_POINT('Ctrl Pts',(17.273341328022,-38.5318258413957,-2.53727755796989));
#7419=CARTESIAN_POINT('Ctrl Pts',(17.2276996951368,-38.587306376714,-2.55469500339263));
#7420=CARTESIAN_POINT('Ctrl Pts',(17.1816263277401,-38.6427404428949,-2.56938903350711));
#7421=CARTESIAN_POINT('Ctrl Pts',(17.1507195756741,-38.6799265014851,-2.57924602402586));
#7422=CARTESIAN_POINT('Ctrl Pts',(17.1196187266954,-38.7170916569447,-2.58787857636224));
#7423=CARTESIAN_POINT('Ctrl Pts',(17.0883919872725,-38.7541583495962,-2.59528770975726));
#7424=CARTESIAN_POINT('Ctrl Pts',(17.0418424025962,-38.8094135308972,-2.6063324774379));
#7425=CARTESIAN_POINT('Ctrl Pts',(16.9948202613371,-38.8653223022424,-2.61475432517947));
#7426=CARTESIAN_POINT('Ctrl Pts',(16.9475382801287,-38.9216337778016,-2.62045518191377));
#7427=CARTESIAN_POINT('Ctrl Pts',(16.9003188246654,-38.9778707870022,-2.6261484998287));
#7428=CARTESIAN_POINT('Ctrl Pts',(16.8528406543402,-39.0345089202757,-2.62912778112529));
#7429=CARTESIAN_POINT('Ctrl Pts',(16.8053254831534,-39.0912848593564,-2.62934454720093));
#7430=CARTESIAN_POINT('Ctrl Pts',(16.7578072923443,-39.1480644065877,-2.62956132705221));
#7431=CARTESIAN_POINT('Ctrl Pts',(16.7102525630312,-39.2049812221505,-2.62701514692948));
#7432=CARTESIAN_POINT('Ctrl Pts',(16.6628860880204,-39.2617665554037,-2.62170927404791));
#7433=CARTESIAN_POINT('Ctrl Pts',(16.615531072387,-39.3185381505741,-2.61640468481683));
#7434=CARTESIAN_POINT('Ctrl Pts',(16.5683646880065,-39.3751777652676,-2.60834181054544));
#7435=CARTESIAN_POINT('Ctrl Pts',(16.5216075573414,-39.4314198750157,-2.59757579979095));
#7436=CARTESIAN_POINT('Ctrl Pts',(16.4747793597799,-39.4877474680289,-2.58679342560781));
#7437=CARTESIAN_POINT('Ctrl Pts',(16.428362104895,-39.5436758089174,-2.57329990897825));
#7438=CARTESIAN_POINT('Ctrl Pts',(16.3825665243119,-39.5989494948066,-2.55720053492649));
#7439=CARTESIAN_POINT('Ctrl Pts',(16.3518461160844,-39.636027967732,-2.54640081720745));
#7440=CARTESIAN_POINT('Ctrl Pts',(16.3214052187708,-39.6728120999206,-2.5344295208121));
#7441=CARTESIAN_POINT('Ctrl Pts',(16.2913032640389,-39.7092293978285,-2.52133001886304));
#7442=CARTESIAN_POINT('Ctrl Pts',(16.2464303917323,-39.7635165287916,-2.50180263987793));
#7443=CARTESIAN_POINT('Ctrl Pts',(16.2021336618314,-39.8178517831556,-2.47959273545151));
#7444=CARTESIAN_POINT('Ctrl Pts',(16.1586360840022,-39.8719783324052,-2.45474630344385));
#7445=CARTESIAN_POINT('Ctrl Pts',(16.115196027419,-39.926033304645,-2.4299327283859));
#7446=CARTESIAN_POINT('Ctrl Pts',(16.0725534835297,-39.979879587694,-2.40248965698983));
#7447=CARTESIAN_POINT('Ctrl Pts',(16.0309206233939,-40.033259372906,-2.37251384629885));
#7448=CARTESIAN_POINT('Ctrl Pts',(15.9892851174606,-40.086642550441,-2.34253613062394));
#7449=CARTESIAN_POINT('Ctrl Pts',(15.9486598673673,-40.139558629311,-2.31002556527922));
#7450=CARTESIAN_POINT('Ctrl Pts',(15.9092402176412,-40.1917558608472,-2.27512786406301));
#7451=CARTESIAN_POINT('Ctrl Pts',(15.8698301047161,-40.2439404643002,-2.24023860565226));
#7452=CARTESIAN_POINT('Ctrl Pts',(15.8316253907928,-40.295406056143,-2.2029637293948));
#7453=CARTESIAN_POINT('Ctrl Pts',(15.794798203504,-40.3459151104098,-2.16349342564628));
#7454=CARTESIAN_POINT('Ctrl Pts',(15.7579150419953,-40.396500934181,-2.12396313036366));
#7455=CARTESIAN_POINT('Ctrl Pts',(15.722413903991,-40.4461268520502,-2.08223120813708));
#7456=CARTESIAN_POINT('Ctrl Pts',(15.6884393559485,-40.4945756616201,-2.03852710839551));
#7457=CARTESIAN_POINT('Ctrl Pts',(15.6656486854977,-40.5270758983049,-2.00920969898324));
#7458=CARTESIAN_POINT('Ctrl Pts',(15.6435443696794,-40.5590469029225,-1.97900561592617));
#7459=CARTESIAN_POINT('Ctrl Pts',(15.6221620196843,-40.5904299346879,-1.94799199564958));
#7460=CARTESIAN_POINT('Ctrl Pts',(15.5902874298272,-40.6372125037797,-1.90176010689442));
#7461=CARTESIAN_POINT('Ctrl Pts',(15.5599562245427,-40.6834847587469,-1.8533173942584));
#7462=CARTESIAN_POINT('Ctrl Pts',(15.5313465526731,-40.729015771483,-1.80284481408956));
#7463=CARTESIAN_POINT('Ctrl Pts',(15.5027747142659,-40.7744865739564,-1.75243897891762));
#7464=CARTESIAN_POINT('Ctrl Pts',(15.4759202503206,-40.8192176047997,-1.70000899168622));
#7465=CARTESIAN_POINT('Ctrl Pts',(15.4509321610801,-40.8629875270547,-1.64577768116532));
#7466=CARTESIAN_POINT('Ctrl Pts',(15.4259424838289,-40.906760230919,-1.59154292420647));
#7467=CARTESIAN_POINT('Ctrl Pts',(15.4028197265874,-40.9495712408294,-1.53550708982251));
#7468=CARTESIAN_POINT('Ctrl Pts',(15.3816791769778,-40.9912150289926,-1.47792947799012));
#7469=CARTESIAN_POINT('Ctrl Pts',(15.3605437419042,-41.0328487422688,-1.42036579591683));
#7470=CARTESIAN_POINT('Ctrl Pts',(15.3413897506042,-41.0733153942767,-1.36126166406269));
#7471=CARTESIAN_POINT('Ctrl Pts',(15.3242948958371,-41.1124319810503,-1.30090464504928));
#7472=CARTESIAN_POINT('Ctrl Pts',(15.3071740583319,-41.1516080217382,-1.24045588845528));
#7473=CARTESIAN_POINT('Ctrl Pts',(15.2921187052635,-41.1894295601709,-1.17875107963721));
#7474=CARTESIAN_POINT('Ctrl Pts',(15.2791671350192,-41.2257407478499,-1.11609838715543));
#7475=CARTESIAN_POINT('Ctrl Pts',(15.2704790144623,-41.2500988735576,-1.07406995853756));
#7476=CARTESIAN_POINT('Ctrl Pts',(15.2627367477603,-41.2737779452521,-1.03161537789602));
#7477=CARTESIAN_POINT('Ctrl Pts',(15.255941797888,-41.2967389376301,-0.988830267143717));
#7478=CARTESIAN_POINT('Ctrl Pts',(15.2458125913074,-41.3309668038336,-0.92505066118307));
#7479=CARTESIAN_POINT('Ctrl Pts',(15.2379209804708,-41.364283552906,-0.859969813685587));
#7480=CARTESIAN_POINT('Ctrl Pts',(15.2323539847774,-41.396510870349,-0.793867798863232));
#7481=CARTESIAN_POINT('Ctrl Pts',(15.2267943508853,-41.4286955703515,-0.727853197418737));
#7482=CARTESIAN_POINT('Ctrl Pts',(15.223553397531,-41.4597933344992,-0.660820696333327));
#7483=CARTESIAN_POINT('Ctrl Pts',(15.2226758380192,-41.4896430359255,-0.5930750621331));
#7484=CARTESIAN_POINT('Ctrl Pts',(15.221798222738,-41.5194946343209,-0.52532512265114));
#7485=CARTESIAN_POINT('Ctrl Pts',(15.2232843886165,-41.5480976758437,-0.4568626034616));
#7486=CARTESIAN_POINT('Ctrl Pts',(15.2271348139984,-41.5753129178684,-0.388009033178963));
#7487=CARTESIAN_POINT('Ctrl Pts',(15.2309843078464,-41.6025215757062,-0.319172120649359));
#7488=CARTESIAN_POINT('Ctrl Pts',(15.2371968620786,-41.6283428458228,-0.249945031376208));
#7489=CARTESIAN_POINT('Ctrl Pts',(15.2457284985217,-41.6526639709981,-0.180655744943154));
#7490=CARTESIAN_POINT('Ctrl Pts',(15.2542731023327,-41.6770220622331,-0.111261144636752));
#7491=CARTESIAN_POINT('Ctrl Pts',(15.265143663798,-41.6998752669307,-0.0418048433736956));
#7492=CARTESIAN_POINT('Ctrl Pts',(15.2782531580267,-41.7211400920208,0.0273873077172026));
#7493=CARTESIAN_POINT('Ctrl Pts',(15.2870472165189,-41.7354048769474,0.0738025098054051));
#7494=CARTESIAN_POINT('Ctrl Pts',(15.2968478865887,-41.7489555293734,0.120098937661456));
#7495=CARTESIAN_POINT('Ctrl Pts',(15.3076189187291,-41.7617747973069,0.166181422977352));
#7496=CARTESIAN_POINT('Ctrl Pts',(15.3236752564046,-41.780884432485,0.234876412976531));
#7497=CARTESIAN_POINT('Ctrl Pts',(15.3422528729634,-41.7989191659951,0.30370533532348));
#7498=CARTESIAN_POINT('Ctrl Pts',(15.3633194390461,-41.8157695893768,0.37234447007484));
#7499=CARTESIAN_POINT('Ctrl Pts',(15.3843581466785,-41.8325977297399,0.440892836358044));
#7500=CARTESIAN_POINT('Ctrl Pts',(15.4078791891891,-41.8482444483706,0.509251242355893));
#7501=CARTESIAN_POINT('Ctrl Pts',(15.4338025321307,-41.8626206415506,0.577093346534493));
#7502=CARTESIAN_POINT('Ctrl Pts',(15.4597275225189,-41.8769977483476,0.644939762126132));
#7503=CARTESIAN_POINT('Ctrl Pts',(15.4880549427528,-41.8901039844429,0.712269124557562));
#7504=CARTESIAN_POINT('Ctrl Pts',(15.5186584489096,-41.9018733280804,0.778761359261807));
#7505=CARTESIAN_POINT('Ctrl Pts',(15.5492545511562,-41.9136398243591,0.845237507490883));
#7506=CARTESIAN_POINT('Ctrl Pts',(15.5821253183861,-41.9240699680251,0.910876280136906));
#7507=CARTESIAN_POINT('Ctrl Pts',(15.6171019638546,-41.9331230601206,0.975374241033202));
#7508=CARTESIAN_POINT('Ctrl Pts',(15.6521317708756,-41.9421899121529,1.03997023339279));
#7509=CARTESIAN_POINT('Ctrl Pts',(15.6892734311379,-41.9498754908882,1.10342135481053));
#7510=CARTESIAN_POINT('Ctrl Pts',(15.7283203630771,-41.9561653293342,1.16544861040137));
#7511=CARTESIAN_POINT('Ctrl Pts',(15.7545136698089,-41.960384653607,1.2070574859452));
#7512=CARTESIAN_POINT('Ctrl Pts',(15.7815635705291,-41.9639764580745,1.24802618569434));
#7513=CARTESIAN_POINT('Ctrl Pts',(15.8094000084028,-41.9669430094149,1.28827884419633));
#7514=CARTESIAN_POINT('Ctrl Pts',(15.8508956831299,-41.9713652364986,1.34828333297729));
#7515=CARTESIAN_POINT('Ctrl Pts',(15.8947296049228,-41.9748182353834,1.4072279179729));
#7516=CARTESIAN_POINT('Ctrl Pts',(15.9407455148334,-41.9772641483903,1.46480935021334));
#7517=CARTESIAN_POINT('Ctrl Pts',(15.9867005732529,-41.9797068269191,1.522314636703));
#7518=CARTESIAN_POINT('Ctrl Pts',(16.0348315554068,-41.981144990272,1.57845972694531));
#7519=CARTESIAN_POINT('Ctrl Pts',(16.0849379261041,-41.9815591058674,1.63296134034162));
#7520=CARTESIAN_POINT('Ctrl Pts',(16.1350474810962,-41.9819732477801,1.68746641735353));
#7521=CARTESIAN_POINT('Ctrl Pts',(16.1871322473098,-41.9813631737787,1.74032721705703));
#7522=CARTESIAN_POINT('Ctrl Pts',(16.2409521642729,-41.9797285163876,1.79128851362614));
#7523=CARTESIAN_POINT('Ctrl Pts',(16.2947590605767,-41.9780942544694,1.84223748112241));
#7524=CARTESIAN_POINT('Ctrl Pts',(16.3502997222452,-41.9754359284791,1.89128737321299));
#7525=CARTESIAN_POINT('Ctrl Pts',(16.4073021361913,-41.9717724372151,1.93821939640231));
#7526=CARTESIAN_POINT('Ctrl Pts',(16.4643911890006,-41.9681033777532,1.98522275230988));
#7527=CARTESIAN_POINT('Ctrl Pts',(16.5229458190129,-41.9634261726391,2.03010142110802));
#7528=CARTESIAN_POINT('Ctrl Pts',(16.5826693342596,-41.9577783801464,2.07267852251417));
#7529=CARTESIAN_POINT('Ctrl Pts',(16.6227328239181,-41.9539897505724,2.10123992341013));
#7530=CARTESIAN_POINT('Ctrl Pts',(16.6633218274874,-41.9497647503652,2.12876654161633));
#7531=CARTESIAN_POINT('Ctrl Pts',(16.7043430819143,-41.945119044319,2.15521684061908));
#7532=CARTESIAN_POINT('Ctrl Pts',(16.7654933137908,-41.9381937075413,2.19464620327067));
#7533=CARTESIAN_POINT('Ctrl Pts',(16.8283682976551,-41.9306533441131,2.23203175294738));
#7534=CARTESIAN_POINT('Ctrl Pts',(16.8927078099147,-41.9225201203709,2.26715077383057));
#7535=CARTESIAN_POINT('Ctrl Pts',(16.9569622395323,-41.9143976520127,2.30222335328179));
#7536=CARTESIAN_POINT('Ctrl Pts',(17.0226768047408,-41.9056839289559,2.33503490407215));
#7537=CARTESIAN_POINT('Ctrl Pts',(17.089558583264,-41.8964127583274,2.36540131373498));
#7538=CARTESIAN_POINT('Ctrl Pts',(17.1564446121707,-41.8871409985096,2.39576965320428));
#7539=CARTESIAN_POINT('Ctrl Pts',(17.2244973822525,-41.8773117931766,2.42369216050363));
#7540=CARTESIAN_POINT('Ctrl Pts',(17.2933987451626,-41.8669698589084,2.44902900915302));
#7541=CARTESIAN_POINT('Ctrl Pts',(17.3622834387564,-41.8566304266658,2.47435972805509));
#7542=CARTESIAN_POINT('Ctrl Pts',(17.4320156256809,-41.8457786197484,2.49710580690362));
#7543=CARTESIAN_POINT('Ctrl Pts',(17.50226209398,-41.8344686701383,2.5171764296093));
#7544=CARTESIAN_POINT('Ctrl Pts',(17.5726153309896,-41.8231415303581,2.53727755796966));
#7545=CARTESIAN_POINT('Ctrl Pts',(17.643483700434,-41.8113549844685,2.55469500339256));
#7546=CARTESIAN_POINT('Ctrl Pts',(17.7145276936807,-41.7991713109554,2.56938903350715));
#7547=CARTESIAN_POINT('Ctrl Pts',(17.7621851411193,-41.7909983078129,2.57924602402589));
#7548=CARTESIAN_POINT('Ctrl Pts',(17.8099215343723,-41.7826467602478,2.58787857636225));
#7549=CARTESIAN_POINT('Ctrl Pts',(17.8576356015541,-41.774136956956,2.59528770975727));
#7550=CARTESIAN_POINT('Ctrl Pts',(17.9287627845899,-41.7614514247412,2.60633247743795));
#7551=CARTESIAN_POINT('Ctrl Pts',(18.000692271499,-41.7486834415431,2.61475432517955));
#7552=CARTESIAN_POINT('Ctrl Pts',(18.0731004304624,-41.7358917824549,2.62045518191384));
#7553=CARTESIAN_POINT('Ctrl Pts',(18.1454128367952,-41.723117039071,2.6261484998288));
#7554=CARTESIAN_POINT('Ctrl Pts',(18.2182019841964,-41.7103188040807,2.62912778112538));
#7555=CARTESIAN_POINT('Ctrl Pts',(18.291128975358,-41.6975574283081,2.62934454720094));
#7556=CARTESIAN_POINT('Ctrl Pts',(18.3640606010804,-41.6847952415412,2.62956132705215));
#7557=CARTESIAN_POINT('Ctrl Pts',(18.437129373917,-41.6720700456673,2.62701514692934));
#7558=CARTESIAN_POINT('Ctrl Pts',(18.5099901525822,-41.6594421416469,2.62170927404767));
#7559=CARTESIAN_POINT('Ctrl Pts',(18.5828333040297,-41.6468172926969,2.61640468481653));
#7560=CARTESIAN_POINT('Ctrl Pts',(18.6554678414049,-41.6342898129655,2.60834181054508));
#7561=CARTESIAN_POINT('Ctrl Pts',(18.7275535025415,-41.6219180048756,2.59757579979054));
#7562=CARTESIAN_POINT('Ctrl Pts',(18.7997487278061,-41.6095273926804,2.58679342560727));
#7563=CARTESIAN_POINT('Ctrl Pts',(18.8713927192498,-41.5972930412203,2.57329990897757));
#7564=CARTESIAN_POINT('Ctrl Pts',(18.9421589256826,-41.5852697479988,2.55720053492563));
#7565=CARTESIAN_POINT('Ctrl Pts',(18.989630029282,-41.5772043305221,2.54640081720681));
#7566=CARTESIAN_POINT('Ctrl Pts',(19.036706470869,-41.569233806229,2.53442952081175));
#7567=CARTESIAN_POINT('Ctrl Pts',(19.0832957533591,-41.5613733976818,2.52133001886304));
#7568=CARTESIAN_POINT('Ctrl Pts',(19.1527462240253,-41.549655915805,2.50180263987786));
#7569=CARTESIAN_POINT('Ctrl Pts',(19.2219502995763,-41.5384614495882,2.47959273545134));
#7570=CARTESIAN_POINT('Ctrl Pts',(19.2905740551605,-41.5278547168098,2.45474630344356));
#7571=CARTESIAN_POINT('Ctrl Pts',(19.3591070626122,-41.5172620103869,2.42993272838577));
#7572=CARTESIAN_POINT('Ctrl Pts',(19.4270605835762,-41.5072556256214,2.40248965698989));
#7573=CARTESIAN_POINT('Ctrl Pts',(19.4941052636857,-41.4978904037176,2.37251384629913));
#7574=CARTESIAN_POINT('Ctrl Pts',(19.5611542045323,-41.4885245866474,2.3425361306243));
#7575=CARTESIAN_POINT('Ctrl Pts',(19.6272934981489,-41.4798001274666,2.31002556527966));
#7576=CARTESIAN_POINT('Ctrl Pts',(19.6922074515294,-41.4717603251636,2.27512786406354));
#7577=CARTESIAN_POINT('Ctrl Pts',(19.7571057002683,-41.4637224679311,2.24023860565303));
#7578=CARTESIAN_POINT('Ctrl Pts',(19.8207785671862,-41.4563690110505,2.20296372939584));
#7579=CARTESIAN_POINT('Ctrl Pts',(19.8829342849465,-41.449730258442,2.16349342564761));
#7580=CARTESIAN_POINT('Ctrl Pts',(19.9451844741582,-41.4430814154891,2.12396313036491));
#7581=CARTESIAN_POINT('Ctrl Pts',(20.0059123487215,-41.4371494870487,2.08223120813824));
#7582=CARTESIAN_POINT('Ctrl Pts',(20.0648575226136,-41.4319510701467,2.03852710839656));
#7583=CARTESIAN_POINT('Ctrl Pts',(20.1043988884376,-41.4284638889094,2.00920969898396));
#7584=CARTESIAN_POINT('Ctrl Pts',(20.1431387485306,-41.4253064921863,1.97900561592653));
#7585=CARTESIAN_POINT('Ctrl Pts',(20.1810084262852,-41.4224803497805,1.94799199564958));
#7586=CARTESIAN_POINT('Ctrl Pts',(20.2374606145016,-41.418267429775,1.90176010689434));
#7587=CARTESIAN_POINT('Ctrl Pts',(20.2926991654359,-41.4151359629548,1.85331739425825));
#7588=CARTESIAN_POINT('Ctrl Pts',(20.3464350150602,-41.4131247666898,1.80284481408933));
#7589=CARTESIAN_POINT('Ctrl Pts',(20.4000998043366,-41.4111162300331,1.75243897891717));
#7590=CARTESIAN_POINT('Ctrl Pts',(20.4522652453572,-41.4102250974731,1.70000899168553));
#7591=CARTESIAN_POINT('Ctrl Pts',(20.5026651545721,-41.4104697385263,1.64577768116439));
#7592=CARTESIAN_POINT('Ctrl Pts',(20.5530682667365,-41.4107143951265,1.59154292420549));
#7593=CARTESIAN_POINT('Ctrl Pts',(20.6017050675013,-41.4120950049051,1.5355070898215));
#7594=CARTESIAN_POINT('Ctrl Pts',(20.6483399207653,-41.4146086459749,1.47792947798907));
#7595=CARTESIAN_POINT('Ctrl Pts',(20.6949634916534,-41.4171216789191,1.42036579591542));
#7596=CARTESIAN_POINT('Ctrl Pts',(20.7395856359485,-41.4207671618734,1.36126166406089));
#7597=CARTESIAN_POINT('Ctrl Pts',(20.7820090211876,-41.425520876758,1.30090464504709));
#7598=CARTESIAN_POINT('Ctrl Pts',(20.8244968863956,-41.4302818168884,1.24045588845307));
#7599=CARTESIAN_POINT('Ctrl Pts',(20.8647789760227,-41.4361542678846,1.17875107963501));
#7600=CARTESIAN_POINT('Ctrl Pts',(20.9027011721163,-41.4430934728737,1.11609838715323));
#7601=CARTESIAN_POINT('Ctrl Pts',(20.9281399880457,-41.4477484026141,1.07406995853608));
#7602=CARTESIAN_POINT('Ctrl Pts',(20.9525177990217,-41.4528829388144,1.03161537789526));
#7603=CARTESIAN_POINT('Ctrl Pts',(20.9758000766529,-41.4584788357964,0.988830267143709));
#7604=CARTESIAN_POINT('Ctrl Pts',(21.0105068815928,-41.4668206186793,0.925050661182975));
#7605=CARTESIAN_POINT('Ctrl Pts',(21.0433058380794,-41.4766446577542,0.85996981368539));
#7606=CARTESIAN_POINT('Ctrl Pts',(21.0739990115276,-41.4879371567824,0.793867798862945));
#7607=CARTESIAN_POINT('Ctrl Pts',(21.1046515962888,-41.4992147225973,0.72785319741889));
#7608=CARTESIAN_POINT('Ctrl Pts',(21.1332035267186,-41.5119568567338,0.660820696333936));
#7609=CARTESIAN_POINT('Ctrl Pts',(21.1594929062049,-41.5261217186163,0.593075062134168));
#7610=CARTESIAN_POINT('Ctrl Pts',(21.1857839563995,-41.5402874806857,0.525325122652251));
#7611=CARTESIAN_POINT('Ctrl Pts',(21.2098118340445,-41.5558760588521,0.456862603462757));
#7612=CARTESIAN_POINT('Ctrl Pts',(21.2314557123171,-41.5728182460605,0.388009033180158));
#7613=CARTESIAN_POINT('Ctrl Pts',(21.2530943542834,-41.5897563344434,0.319172120650899));
#7614=CARTESIAN_POINT('Ctrl Pts',(21.2723499530461,-41.6080471992891,0.249945031378103));
#7615=CARTESIAN_POINT('Ctrl Pts',(21.2891468470751,-41.6275963757721,0.180655744945393));
#7616=CARTESIAN_POINT('Ctrl Pts',(21.3059692709667,-41.6471752653552,0.111261144639139));
#7617=CARTESIAN_POINT('Ctrl Pts',(21.3203254460601,-41.6680160500862,0.0418048433762189));
#7618=CARTESIAN_POINT('Ctrl Pts',(21.3321865776809,-41.690001617664,-0.0273873077145389));
#7619=CARTESIAN_POINT('Ctrl Pts',(21.3401432145609,-41.7047498881843,-0.0738025098036383));
#7620=CARTESIAN_POINT('Ctrl Pts',(21.346978088765,-41.7200128436521,-0.120098937660575));
#7621=CARTESIAN_POINT('Ctrl Pts',(21.3526943843832,-41.7357504650777,-0.166181422977357));
#7622=CARTESIAN_POINT('Ctrl Pts',(21.3612156450668,-41.7592104789858,-0.234876412977378));
#7623=CARTESIAN_POINT('Ctrl Pts',(21.3675453741577,-41.7843165336228,-0.303705335325169));
#7624=CARTESIAN_POINT('Ctrl Pts',(21.3716049858294,-41.8109859267122,-0.372344470077365));
#7625=CARTESIAN_POINT('Ctrl Pts',(21.3756592290661,-41.837620052166,-0.440892836360022));
#7626=CARTESIAN_POINT('Ctrl Pts',(21.3774491636307,-41.8658132318188,-0.509251242357337));
#7627=CARTESIAN_POINT('Ctrl Pts',(21.3769376406635,-41.8954516019471,-0.577093346535395));
#7628=CARTESIAN_POINT('Ctrl Pts',(21.3764260851885,-41.9250918556145,-0.644939762126841));
#7629=CARTESIAN_POINT('Ctrl Pts',(21.373612708478,-41.9561772392083,-0.712269124558073));
#7630=CARTESIAN_POINT('Ctrl Pts',(21.3685035059756,-41.9885653248037,-0.77876135926213));
#7631=CARTESIAN_POINT('Ctrl Pts',(21.3633955395432,-42.0209455747454,-0.845237507491449));
#7632=CARTESIAN_POINT('Ctrl Pts',(21.3559929253081,-42.0546275660416,-0.910876280137711));
#7633=CARTESIAN_POINT('Ctrl Pts',(21.3463448103113,-42.0894447756044,-0.975374241034235));
#7634=CARTESIAN_POINT('Ctrl Pts',(21.3366820309931,-42.1243149043904,-1.03997023339384));
#7635=CARTESIAN_POINT('Ctrl Pts',(21.3247671072895,-42.160323315084,-1.1034213548116));
#7636=CARTESIAN_POINT('Ctrl Pts',(21.3106908011998,-42.1972838693061,-1.16544861040246));
#7637=CARTESIAN_POINT('Ctrl Pts',(21.301248189841,-42.2220776004812,-1.20705748594591));
#7638=CARTESIAN_POINT('Ctrl Pts',(21.2908338333953,-42.2472994039083,-1.24802618569469));
#7639=CARTESIAN_POINT('Ctrl Pts',(21.2794847232809,-42.2728897419278,-1.28827884419633));
#7640=CARTESIAN_POINT('Ctrl Pts',(21.2625666469131,-42.3110371639306,-1.34828333297748));
#7641=CARTESIAN_POINT('Ctrl Pts',(21.24364007077,-42.3507249531932,-1.40722791797326));
#7642=CARTESIAN_POINT('Ctrl Pts',(21.2227503386141,-42.3917988566577,-1.46480935021387));
#7643=CARTESIAN_POINT('Ctrl Pts',(21.2018882310633,-42.4328184439464,-1.52231463670436));
#7644=CARTESIAN_POINT('Ctrl Pts',(21.1790682259843,-42.4752201788778,-1.57845972694747));
#7645=CARTESIAN_POINT('Ctrl Pts',(21.154373675261,-42.5188206265915,-1.63296134034452));
#7646=CARTESIAN_POINT('Ctrl Pts',(21.129677555182,-42.5624238451434,-1.68746641735642));
#7647=CARTESIAN_POINT('Ctrl Pts',(21.1031068324917,-42.607225538834,-1.74032721705991));
#7648=CARTESIAN_POINT('Ctrl Pts',(21.0747812191829,-42.6530176254581,-1.79128851362901));
#7649=CARTESIAN_POINT('Ctrl Pts',(21.0464624586933,-42.6987986335969,-1.84223748112507));
#7650=CARTESIAN_POINT('Ctrl Pts',(21.01638995002,-42.7455690945495,-1.89128737321547));
#7651=CARTESIAN_POINT('Ctrl Pts',(20.9847160665458,-42.7931028874718,-1.9382193964046));
#7652=CARTESIAN_POINT('Ctrl Pts',(20.9529940414388,-42.8407089277522,-1.98522275231258));
#7653=CARTESIAN_POINT('Ctrl Pts',(20.9196661479847,-42.8890801222955,-2.03010142111108));
#7654=CARTESIAN_POINT('Ctrl Pts',(20.8849132585869,-42.9379783074566,-2.07267852251754));
#7655=CARTESIAN_POINT('Ctrl Pts',(20.8616004643019,-42.9707799924769,-2.1012399234123));
#7656=CARTESIAN_POINT('Ctrl Pts',(20.8376470050078,-43.0038186005773,-2.12876654161737));
#7657=CARTESIAN_POINT('Ctrl Pts',(20.8131130783408,-43.0370211959817,-2.15521684061907));
#7658=CARTESIAN_POINT('Ctrl Pts',(20.7765404448229,-43.0865161818458,-2.19464620327108));
#7659=CARTESIAN_POINT('Ctrl Pts',(20.7385728066078,-43.1371973334212,-2.23203175294819));
#7660=CARTESIAN_POINT('Ctrl Pts',(20.6993594721021,-43.1888503736346,-2.26715077383171));
#7661=CARTESIAN_POINT('Ctrl Pts',(20.6601979933538,-43.2404351078099,-2.30222335328278));
#7662=CARTESIAN_POINT('Ctrl Pts',(20.6197944052208,-43.2929887291506,-2.335034904073));
#7663=CARTESIAN_POINT('Ctrl Pts',(20.5783244466722,-43.3462744630876,-2.36540131373571));
#7664=CARTESIAN_POINT('Ctrl Pts',(20.5368518526788,-43.3995635833702,-2.39576965320497));
#7665=CARTESIAN_POINT('Ctrl Pts',(20.4943131261206,-43.4535844083924,-2.42369216050428));
#7666=CARTESIAN_POINT('Ctrl Pts',(20.450906066865,-43.5080837718938,-2.44902900915362));
#7667=CARTESIAN_POINT('Ctrl Pts',(20.4075095090847,-43.5625699503573,-2.47435972805595));
#7668=CARTESIAN_POINT('Ctrl Pts',(20.3632454751545,-43.6175338922374,-2.49710580690468));
#7669=CARTESIAN_POINT('Ctrl Pts',(20.3183275373265,-43.6727141435061,-2.51717642961049));
#7670=CARTESIAN_POINT('Ctrl Pts',(20.2733413280198,-43.7279782641049,-2.53727755797076));
#7671=CARTESIAN_POINT('Ctrl Pts',(20.2276996951343,-43.7834587994236,-2.55469500339356));
#7672=CARTESIAN_POINT('Ctrl Pts',(20.1816263277371,-43.8388928656051,-2.56938903350804));
#7673=CARTESIAN_POINT('Ctrl Pts',(20.1507195756722,-43.8760789241941,-2.57924602402641));
#7674=CARTESIAN_POINT('Ctrl Pts',(20.1196187266944,-43.9132440796525,-2.58787857636247));
#7675=CARTESIAN_POINT('Ctrl Pts',(20.0883919872725,-43.9503107723028,-2.59528770975726));
#7676=CARTESIAN_POINT('Ctrl Pts',(20.0418424025962,-44.0055659536039,-2.60633247743792));
#7677=CARTESIAN_POINT('Ctrl Pts',(19.994820261337,-44.0614747249492,-2.6147543251795));
#7678=CARTESIAN_POINT('Ctrl Pts',(19.9475382801285,-44.1177862005085,-2.62045518191379));
#7679=CARTESIAN_POINT('Ctrl Pts',(19.9003188246649,-44.1740232097094,-2.62614849982876));
#7680=CARTESIAN_POINT('Ctrl Pts',(19.8528406543392,-44.2306613429835,-2.62912778112535));
#7681=CARTESIAN_POINT('Ctrl Pts',(19.8053254831521,-44.2874372820646,-2.62934454720094));
#7682=CARTESIAN_POINT('Ctrl Pts',(19.7578072923429,-44.3442168292961,-2.62956132705216));
#7683=CARTESIAN_POINT('Ctrl Pts',(19.7102525630296,-44.401133644859,-2.62701514692937));
#7684=CARTESIAN_POINT('Ctrl Pts',(19.6628860880186,-44.4579189781125,-2.62170927404771));
#7685=CARTESIAN_POINT('Ctrl Pts',(19.6155310723851,-44.514690573283,-2.61640468481656));
#7686=CARTESIAN_POINT('Ctrl Pts',(19.5683646880045,-44.5713301879767,-2.60834181054507));
#7687=CARTESIAN_POINT('Ctrl Pts',(19.5216075573393,-44.6275722977249,-2.59757579979048));
#7688=CARTESIAN_POINT('Ctrl Pts',(19.4747793597774,-44.6838998907385,-2.58679342560716));
#7689=CARTESIAN_POINT('Ctrl Pts',(19.4283621048922,-44.7398282316274,-2.57329990897739));
#7690=CARTESIAN_POINT('Ctrl Pts',(19.3825665243087,-44.7951019175171,-2.55720053492538));
#7691=CARTESIAN_POINT('Ctrl Pts',(19.3518461160823,-44.8321803904412,-2.54640081720663));
#7692=CARTESIAN_POINT('Ctrl Pts',(19.3214052187697,-44.8689645226285,-2.53442952081165));
#7693=CARTESIAN_POINT('Ctrl Pts',(19.2913032640389,-44.9053818205351,-2.52133001886304));
#7694=CARTESIAN_POINT('Ctrl Pts',(19.246430467523,-44.9596688598067,-2.5018026728599));
#7695=CARTESIAN_POINT('Ctrl Pts',(19.202133795719,-45.0140040172023,-2.47959281974212));
#7696=CARTESIAN_POINT('Ctrl Pts',(19.1586362574803,-45.068130464348,-2.45474645544533));
#7697=CARTESIAN_POINT('Ctrl Pts',(19.1134700774478,-45.1243332968597,-2.42894694107226));
#7698=CARTESIAN_POINT('Ctrl Pts',(19.0691661346203,-45.1803104983177,-2.40030445526987));
#7699=CARTESIAN_POINT('Ctrl Pts',(19.0259625921186,-45.2357723552297,-2.36892887071559));
#7700=CARTESIAN_POINT('Ctrl Pts',(18.9827590496168,-45.2912342121417,-2.3375532861613));
#7701=CARTESIAN_POINT('Ctrl Pts',(18.9406564439223,-45.3461800674173,-2.30344486801562));
#7702=CARTESIAN_POINT('Ctrl Pts',(18.8998729273403,-45.4003277207435,-2.26677050498056));
#7703=CARTESIAN_POINT('Origin',(5.49999999999995,-19.5262794416289,2.16840434497101E-16));
#7704=CARTESIAN_POINT('',(7.09807621135328,-16.29422863406,-1.50553605247105E-16));
#7705=CARTESIAN_POINT('Origin',(4.49999999999996,-17.79422863406,2.16840434497101E-16));
#7706=CARTESIAN_POINT('',(8.09807621135327,-18.0262794416289,-1.50553605247105E-16));
#7707=CARTESIAN_POINT('',(8.09807621135327,-18.0262794416289,-1.50553605247105E-16));
#7708=CARTESIAN_POINT('Origin',(5.49999999999995,-19.5262794416289,2.16840434497101E-16));
#7709=CARTESIAN_POINT('Origin',(0.,-10.,3.));
#7710=CARTESIAN_POINT('',(1.5,-10.,3.));
#7711=CARTESIAN_POINT('Origin',(0.,-10.,3.));
#7712=CARTESIAN_POINT('',(1.5,-10.,-3.));
#7713=CARTESIAN_POINT('',(1.5,-10.,3.));
#7714=CARTESIAN_POINT('Origin',(0.,-10.,-3.));
#7715=CARTESIAN_POINT('Origin',(0.,-10.,3.));
#7716=CARTESIAN_POINT('',(2.5,-10.,-3.));
#7717=CARTESIAN_POINT('Origin',(0.,-10.,-3.));
#7718=CARTESIAN_POINT('',(2.5,-10.,3.));
#7719=CARTESIAN_POINT('',(2.5,-10.,3.));
#7720=CARTESIAN_POINT('Origin',(0.,-10.,3.));
#7721=CARTESIAN_POINT('',(2.40822301019062,-10.6711646096066,1.));
#7722=CARTESIAN_POINT('',(-0.622865903054925,-12.4211646096066,1.));
#7723=CARTESIAN_POINT('Origin',(0.,-10.,1.));
#7724=CARTESIAN_POINT('',(2.40822301019062,-10.6711646096066,-1.));
#7725=CARTESIAN_POINT('',(2.40822301019062,-10.6711646096066,3.));
#7726=CARTESIAN_POINT('',(-0.622865903054925,-12.4211646096066,-1.));
#7727=CARTESIAN_POINT('Origin',(0.,-10.,-1.));
#7728=CARTESIAN_POINT('',(-0.622865903054925,-12.4211646096066,3.));
#7729=CARTESIAN_POINT('Origin',(-0.76554445662278,-12.1740381056767,1.));
#7730=CARTESIAN_POINT('',(2.98445554337718,-18.66922863406,1.));
#7731=CARTESIAN_POINT('',(2.98445554337718,-18.66922863406,-1.));
#7732=CARTESIAN_POINT('',(2.98445554337718,-18.66922863406,1.));
#7733=CARTESIAN_POINT('',(-0.76554445662278,-12.1740381056767,1.));
#7734=CARTESIAN_POINT('',(-0.76554445662278,-12.1740381056767,-1.));
#7735=CARTESIAN_POINT('Origin',(2.26554445662277,-10.4240381056767,1.));
#7736=CARTESIAN_POINT('',(6.01554445662273,-16.91922863406,1.));
#7737=CARTESIAN_POINT('',(2.26554445662277,-10.4240381056767,1.));
#7738=CARTESIAN_POINT('',(6.01554445662273,-16.91922863406,-1.));
#7739=CARTESIAN_POINT('',(6.01554445662273,-16.91922863406,1.));
#7740=CARTESIAN_POINT('',(2.26554445662277,-10.4240381056767,-1.));
#7741=CARTESIAN_POINT('Origin',(0.,0.,1.));
#7742=CARTESIAN_POINT('',(8.83012701892212,-15.29422863406,1.));
#7743=CARTESIAN_POINT('Origin',(0.,0.,-1.));
#7744=CARTESIAN_POINT('',(8.83012701892212,-15.29422863406,-1.));
#7745=CARTESIAN_POINT('Origin',(0.,-10.,3.));
#7746=CARTESIAN_POINT('Origin',(0.,-10.,-3.));
#7747=CARTESIAN_POINT('Origin',(4.49999999999996,-17.79422863406,2.16840434497101E-16));
#7748=CARTESIAN_POINT('Origin',(5.49999999999995,-19.5262794416289,2.16840434497101E-16));
#7749=CARTESIAN_POINT('Ctrl Pts',(3.23546955922298,-20.8337067011995,-0.275782109461831));
#7750=CARTESIAN_POINT('Ctrl Pts',(3.19478646287985,-20.8571950978247,-0.160590892492083));
#7751=CARTESIAN_POINT('Ctrl Pts',(3.16609800813309,-20.8737583848954,-0.0273286702176377));
#7752=CARTESIAN_POINT('Ctrl Pts',(3.13988678358144,-20.888891442446,0.302695031901609));
#7753=CARTESIAN_POINT('Ctrl Pts',(3.15185977323478,-20.8819788336467,0.505045958749506));
#7754=CARTESIAN_POINT('Ctrl Pts',(3.24434506152257,-20.8285824275577,0.905660854503917));
#7755=CARTESIAN_POINT('Ctrl Pts',(3.31916946032855,-20.7853825407651,1.09246911691544));
#7756=CARTESIAN_POINT('Ctrl Pts',(3.51311377456417,-20.6734087387334,1.40491660680051));
#7757=CARTESIAN_POINT('Ctrl Pts',(3.62398989329116,-20.6093943817396,1.52876642599518));
#7758=CARTESIAN_POINT('Ctrl Pts',(3.81928683300962,-20.4966396410213,1.66967867861614));
#7759=CARTESIAN_POINT('Ctrl Pts',(3.89646793982015,-20.4520791082279,1.70509112652145));
#7760=CARTESIAN_POINT('Ctrl Pts',(4.01069549422891,-20.3861297989411,1.72863250364951));
#7761=CARTESIAN_POINT('Ctrl Pts',(4.05275149332675,-20.3618487565409,1.72894065285834));
#7762=CARTESIAN_POINT('Ctrl Pts',(4.11567773776654,-20.3255182723745,1.71361810977144));
#7763=CARTESIAN_POINT('Ctrl Pts',(4.14030222240021,-20.3113013195102,1.70246840376101));
#7764=CARTESIAN_POINT('Ctrl Pts',(4.18011703938166,-20.2883142242082,1.67084097729165));
#7765=CARTESIAN_POINT('Ctrl Pts',(4.19525068130979,-20.2795768119921,1.65305151274377));
#7766=CARTESIAN_POINT('Ctrl Pts',(4.22086530937756,-20.264788199582,1.60918078140847));
#7767=CARTESIAN_POINT('Ctrl Pts',(4.2301173432281,-20.2594465353219,1.58365589452017));
#7768=CARTESIAN_POINT('Ctrl Pts',(4.24553996400391,-20.2505422810654,1.51733112234353));
#7769=CARTESIAN_POINT('Ctrl Pts',(4.24810838618388,-20.2490594018618,1.47473909891144));
#7770=CARTESIAN_POINT('Ctrl Pts',(4.24563774453512,-20.2504858274828,1.34638123818485));
#7771=CARTESIAN_POINT('Ctrl Pts',(4.22827734454219,-20.2605088590919,1.24517362806592));
#7772=CARTESIAN_POINT('Ctrl Pts',(4.20325688541709,-20.2749544279031,1.13384235805383));
#7773=CARTESIAN_POINT('Origin',(18.6221620196843,-45.0864402030305,-1.2339885196899));
#7774=CARTESIAN_POINT('Ctrl Pts',(18.6886546214932,-45.2109506803708,-1.32333454806873));
#7775=CARTESIAN_POINT('Ctrl Pts',(18.6534200942688,-45.1984263741837,-1.33050220974328));
#7776=CARTESIAN_POINT('Ctrl Pts',(18.6179251635874,-45.1908739234988,-1.34288752657174));
#7777=CARTESIAN_POINT('Ctrl Pts',(18.5470215891454,-45.185850564164,-1.37789046380575));
#7778=CARTESIAN_POINT('Ctrl Pts',(18.5124223059912,-45.1893923862984,-1.40108283157508));
#7779=CARTESIAN_POINT('Ctrl Pts',(18.4521552156851,-45.2081885454495,-1.45435746423492));
#7780=CARTESIAN_POINT('Ctrl Pts',(18.426979600515,-45.2232129895809,-1.48392674358772));
#7781=CARTESIAN_POINT('Ctrl Pts',(18.389723568323,-45.2625315455739,-1.54510765557877));
#7782=CARTESIAN_POINT('Ctrl Pts',(18.3777553489124,-45.2862666614671,-1.57608573045647));
#7783=CARTESIAN_POINT('Ctrl Pts',(18.3679521931281,-45.3419359617658,-1.63840496576467));
#7784=CARTESIAN_POINT('Ctrl Pts',(18.3717657514849,-45.3715611958691,-1.66645854752162));
#7785=CARTESIAN_POINT('Ctrl Pts',(18.3912949388311,-45.4302955552117,-1.71530376490681));
#7786=CARTESIAN_POINT('Ctrl Pts',(18.4084911637847,-45.4596223662212,-1.73547949720297));
#7787=CARTESIAN_POINT('Ctrl Pts',(18.4492950593841,-45.5109364170729,-1.76471771766154));
#7788=CARTESIAN_POINT('Ctrl Pts',(18.4757817897306,-45.5370275164247,-1.77633599562865));
#7789=CARTESIAN_POINT('Ctrl Pts',(18.5261801552888,-45.5734326754053,-1.78494045784658));
#7790=CARTESIAN_POINT('Ctrl Pts',(18.5444289208832,-45.584745828607,-1.78615024656862));
#7791=CARTESIAN_POINT('Ctrl Pts',(18.5825570867818,-45.6048265898968,-1.78505107379611));
#7792=CARTESIAN_POINT('Ctrl Pts',(18.6022265451803,-45.6134733978683,-1.78273773091633));
#7793=CARTESIAN_POINT('Ctrl Pts',(18.6221620188092,-45.6205950572474,-1.77871850142445));
#7794=CARTESIAN_POINT('Ctrl Pts',(18.8143835621595,-45.3725581651887,-2.29264601963605));
#7795=CARTESIAN_POINT('Ctrl Pts',(18.799421862846,-45.366692611081,-2.29601323464502));
#7796=CARTESIAN_POINT('Ctrl Pts',(18.7845100498018,-45.360314232665,-2.29875605009942));
#7797=CARTESIAN_POINT('Ctrl Pts',(18.7622518217144,-45.3499802606706,-2.30191697923756));
#7798=CARTESIAN_POINT('Ctrl Pts',(18.7548376244511,-45.3464005096126,-2.30281208768347));
#7799=CARTESIAN_POINT('Ctrl Pts',(18.7400559460073,-45.3389851193664,-2.30427767151426));
#7800=CARTESIAN_POINT('Ctrl Pts',(18.7326634287054,-45.3351353187089,-2.3048487962336));
#7801=CARTESIAN_POINT('Ctrl Pts',(18.7107560010767,-45.3232997976908,-2.30605306308975));
#7802=CARTESIAN_POINT('Ctrl Pts',(18.69647386335,-45.3150169340706,-2.30618966865469));
#7803=CARTESIAN_POINT('Ctrl Pts',(18.668502415621,-45.297660633993,-2.30516256178937));
#7804=CARTESIAN_POINT('Ctrl Pts',(18.6548195137261,-45.2885911850942,-2.3039990903213));
#7805=CARTESIAN_POINT('Ctrl Pts',(18.6280626028503,-45.269665384442,-2.3003672370976));
#7806=CARTESIAN_POINT('Ctrl Pts',(18.6150036070141,-45.2598211706463,-2.29790262175487));
#7807=CARTESIAN_POINT('Ctrl Pts',(18.5958424864585,-45.244407875027,-2.29318270097683));
#7808=CARTESIAN_POINT('Ctrl Pts',(18.5895683887268,-45.2391944776938,-2.29144761696805));
#7809=CARTESIAN_POINT('Ctrl Pts',(18.5773056208511,-45.2286717796098,-2.28767708876727));
#7810=CARTESIAN_POINT('Ctrl Pts',(18.571302721882,-45.2233510576313,-2.28563816739681));
#7811=CARTESIAN_POINT('Ctrl Pts',(18.5536922471648,-45.2072288630195,-2.27907242657322));
#7812=CARTESIAN_POINT('Ctrl Pts',(18.5424689819436,-45.1962571521417,-2.27409434987581));
#7813=CARTESIAN_POINT('Ctrl Pts',(18.5210534195265,-45.1738767847226,-2.26294902313096));
#7814=CARTESIAN_POINT('Ctrl Pts',(18.5108563517502,-45.1624608434638,-2.2567766707594));
#7815=CARTESIAN_POINT('Ctrl Pts',(18.4915255994775,-45.1392076266336,-2.24323675136636));
#7816=CARTESIAN_POINT('Ctrl Pts',(18.4823425082748,-45.1272886562345,-2.23580916151862));
#7817=CARTESIAN_POINT('Ctrl Pts',(18.4654779188592,-45.1035758058956,-2.22008460131979));
#7818=CARTESIAN_POINT('Ctrl Pts',(18.4577062314804,-45.0916806335816,-2.21173267647811));
#7819=CARTESIAN_POINT('Ctrl Pts',(18.4435024450096,-45.0678731904181,-2.19410226893954));
#7820=CARTESIAN_POINT('Ctrl Pts',(18.4370613768115,-45.0559500756431,-2.18481745164526));
#7821=CARTESIAN_POINT('Ctrl Pts',(18.4283974556018,-45.0380432871124,-2.17018589369896));
#7822=CARTESIAN_POINT('Ctrl Pts',(18.4256747602959,-45.0320672479267,-2.1651880723044));
#7823=CARTESIAN_POINT('Ctrl Pts',(18.4205692543985,-45.0201143102805,-2.15495946376726));
#7824=CARTESIAN_POINT('Ctrl Pts',(18.4181811783317,-45.0141230761169,-2.14971582230565));
#7825=CARTESIAN_POINT('Ctrl Pts',(18.411557743034,-44.996204520912,-2.13367800718911));
#7826=CARTESIAN_POINT('Ctrl Pts',(18.4079107853335,-44.9844773686462,-2.12271082270486));
#7827=CARTESIAN_POINT('Ctrl Pts',(18.4020639448891,-44.9613631523321,-2.10017046144782));
#7828=CARTESIAN_POINT('Ctrl Pts',(18.3998694271457,-44.9499903424353,-2.08860999048261));
#7829=CARTESIAN_POINT('Ctrl Pts',(18.3969224236575,-44.927612616283,-2.06491243172319));
#7830=CARTESIAN_POINT('Ctrl Pts',(18.3961709968481,-44.9166059372197,-2.05277259205872));
#7831=CARTESIAN_POINT('Ctrl Pts',(18.3961415719036,-44.9003846022915,-2.03412910558187));
#7832=CARTESIAN_POINT('Ctrl Pts',(18.3963173860228,-44.8950134660865,-2.02782648667107));
#7833=CARTESIAN_POINT('Ctrl Pts',(18.3970392739734,-44.8844199010087,-2.01513320991302));
#7834=CARTESIAN_POINT('Ctrl Pts',(18.3975826848578,-44.879219163033,-2.00876936719308));
#7835=CARTESIAN_POINT('Ctrl Pts',(18.3997509614153,-44.8639020731823,-1.98962815132851));
#7836=CARTESIAN_POINT('Ctrl Pts',(18.4019103092124,-44.8540407117655,-1.97676890218923));
#7837=CARTESIAN_POINT('Ctrl Pts',(18.407622325662,-44.835045996909,-1.95090394599962));
#7838=CARTESIAN_POINT('Ctrl Pts',(18.4111751980384,-44.825905164125,-1.93788950367134));
#7839=CARTESIAN_POINT('Ctrl Pts',(18.4196773870788,-44.8083449742005,-1.91169905664016));
#7840=CARTESIAN_POINT('Ctrl Pts',(18.4246337291704,-44.7999153918194,-1.89850633451621));
#7841=CARTESIAN_POINT('Ctrl Pts',(18.4359627695104,-44.7838395187261,-1.87201135519203));
#7842=CARTESIAN_POINT('Ctrl Pts',(18.4422430814637,-44.7763186261024,-1.85891858586588));
#7843=CARTESIAN_POINT('Ctrl Pts',(18.4560163442605,-44.7622376811399,-1.83296819839048));
#7844=CARTESIAN_POINT('Ctrl Pts',(18.4635048906187,-44.7556841943707,-1.82012124842252));
#7845=CARTESIAN_POINT('Ctrl Pts',(18.4796749688842,-44.7435444443489,-1.79468113425342));
#7846=CARTESIAN_POINT('Ctrl Pts',(18.4883628415307,-44.737956512423,-1.78208152867849));
#7847=CARTESIAN_POINT('Ctrl Pts',(18.5069294527721,-44.7277745729134,-1.75716664715693));
#7848=CARTESIAN_POINT('Ctrl Pts',(18.5168839026318,-44.7231591454028,-1.74477273547151));
#7849=CARTESIAN_POINT('Ctrl Pts',(18.5375829891438,-44.7151329976084,-1.72079652319878));
#7850=CARTESIAN_POINT('Ctrl Pts',(18.5483955659724,-44.7116778811927,-1.70911489538877));
#7851=CARTESIAN_POINT('Ctrl Pts',(18.5708927433727,-44.7058864158376,-1.68640778762084));
#7852=CARTESIAN_POINT('Ctrl Pts',(18.5825836040364,-44.703545953535,-1.67537312136182));
#7853=CARTESIAN_POINT('Ctrl Pts',(18.6068588448963,-44.6999847326678,-1.65394839029514));
#7854=CARTESIAN_POINT('Ctrl Pts',(18.619445513792,-44.6987636790236,-1.64355633794861));
#7855=CARTESIAN_POINT('Ctrl Pts',(18.645538711709,-44.6974830389479,-1.6234501769643));
#7856=CARTESIAN_POINT('Ctrl Pts',(18.6588325169338,-44.6974335055609,-1.61389957814289));
#7857=CARTESIAN_POINT('Ctrl Pts',(18.6859142215439,-44.6984777777184,-1.59576518307013));
#7858=CARTESIAN_POINT('Ctrl Pts',(18.6997000237853,-44.6995718128947,-1.58718313777874));
#7859=CARTESIAN_POINT('Ctrl Pts',(18.7277631107646,-44.7028992757828,-1.57098989163726));
#7860=CARTESIAN_POINT('Ctrl Pts',(18.7420482463831,-44.705135147643,-1.56337590956548));
#7861=CARTESIAN_POINT('Ctrl Pts',(18.7710946722565,-44.7107644468085,-1.54915862669876));
#7862=CARTESIAN_POINT('Ctrl Pts',(18.7859459094799,-44.7141859522031,-1.54252376800531));
#7863=CARTESIAN_POINT('Ctrl Pts',(18.8156397942149,-44.7221041428292,-1.53052427124137));
#7864=CARTESIAN_POINT('Ctrl Pts',(18.8305728440077,-44.7266157346991,-1.52511234349085));
#7865=CARTESIAN_POINT('Ctrl Pts',(18.860539209484,-44.7367266946174,-1.5155044665792));
#7866=CARTESIAN_POINT('Ctrl Pts',(18.8756508883745,-44.7423612795317,-1.51129385304441));
#7867=CARTESIAN_POINT('Ctrl Pts',(18.9054576403702,-44.7545267829697,-1.50424311881235));
#7868=CARTESIAN_POINT('Ctrl Pts',(18.9202547119906,-44.7610889823919,-1.50136656793277));
#7869=CARTESIAN_POINT('Ctrl Pts',(18.9495825981467,-44.7751396990536,-1.49691920365679));
#7870=CARTESIAN_POINT('Ctrl Pts',(18.9641293094195,-44.7826350228748,-1.49534501613366));
#7871=CARTESIAN_POINT('Ctrl Pts',(18.9857447788442,-44.7945759268798,-1.49397586706081));
#7872=CARTESIAN_POINT('Ctrl Pts',(18.9929278602255,-44.7986804211822,-1.49368555779672));
#7873=CARTESIAN_POINT('Ctrl Pts',(19.0072126126538,-44.8071190824507,-1.49344249033367));
#7874=CARTESIAN_POINT('Ctrl Pts',(19.0143424710875,-44.8114714840967,-1.49349117220706));
#7875=CARTESIAN_POINT('Ctrl Pts',(19.0354329844958,-44.8247714038735,-1.49415091340346));
#7876=CARTESIAN_POINT('Ctrl Pts',(19.0491062136184,-44.8339600939764,-1.49526534883766));
#7877=CARTESIAN_POINT('Ctrl Pts',(19.0757504934149,-44.8529989681212,-1.49881561860667));
#7878=CARTESIAN_POINT('Ctrl Pts',(19.0887128011736,-44.8628432034342,-1.50125064598544));
#7879=CARTESIAN_POINT('Ctrl Pts',(19.1139155845031,-44.8831828996875,-1.50744605367826));
#7880=CARTESIAN_POINT('Ctrl Pts',(19.1261415989452,-44.8936651252513,-1.51120097784455));
#7881=CARTESIAN_POINT('Ctrl Pts',(19.1439645943469,-44.9099328769387,-1.51787676636393));
#7882=CARTESIAN_POINT('Ctrl Pts',(19.1497815019618,-44.9154129298509,-1.5202634684245));
#7883=CARTESIAN_POINT('Ctrl Pts',(19.1611066834579,-44.9264248357533,-1.52532718281113));
#7884=CARTESIAN_POINT('Ctrl Pts',(19.1666295883308,-44.9319700105026,-1.52800963496645));
#7885=CARTESIAN_POINT('Ctrl Pts',(19.182766450003,-44.9487031839457,-1.53649330236943));
#7886=CARTESIAN_POINT('Ctrl Pts',(19.1929633751574,-44.9600013145975,-1.54273516166076));
#7887=CARTESIAN_POINT('Ctrl Pts',(19.2122406126713,-44.9828745059678,-1.55637255063521));
#7888=CARTESIAN_POINT('Ctrl Pts',(19.2213264422722,-44.9944588868497,-1.56377534127668));
#7889=CARTESIAN_POINT('Ctrl Pts',(19.2383462415657,-45.0178815598089,-1.5797264080401));
#7890=CARTESIAN_POINT('Ctrl Pts',(19.2463304771073,-45.0298136028999,-1.58835146880908));
#7891=CARTESIAN_POINT('Ctrl Pts',(19.2607714831931,-45.0534013484058,-1.60637132681278));
#7892=CARTESIAN_POINT('Ctrl Pts',(19.2673038350586,-45.0651515570016,-1.61582546123857));
#7893=CARTESIAN_POINT('Ctrl Pts',(19.2789889194292,-45.0885216379426,-1.63556445143045));
#7894=CARTESIAN_POINT('Ctrl Pts',(19.2841483413751,-45.1001499111597,-1.64585461771952));
#7895=CARTESIAN_POINT('Ctrl Pts',(19.2930976235061,-45.1232965562804,-1.66727425622956));
#7896=CARTESIAN_POINT('Ctrl Pts',(19.2968886296023,-45.1348186371361,-1.67840737565011));
#7897=CARTESIAN_POINT('Ctrl Pts',(19.3030533575681,-45.1577395162296,-1.70152165051547));
#7898=CARTESIAN_POINT('Ctrl Pts',(19.3053753002664,-45.1689424569227,-1.71330457990983));
#7899=CARTESIAN_POINT('Ctrl Pts',(19.3085649502556,-45.1908773666279,-1.73731958680616));
#7900=CARTESIAN_POINT('Ctrl Pts',(19.3094315307921,-45.2016060723277,-1.74954856369043));
#7901=CARTESIAN_POINT('Ctrl Pts',(19.3097256320476,-45.2225959572621,-1.77444163318775));
#7902=CARTESIAN_POINT('Ctrl Pts',(19.3091504322929,-45.2328640131764,-1.78711583153893));
#7903=CARTESIAN_POINT('Ctrl Pts',(19.3065477416738,-45.2529009468769,-1.81286399012433));
#7904=CARTESIAN_POINT('Ctrl Pts',(19.3044916971078,-45.2627436719468,-1.82604582345194));
#7905=CARTESIAN_POINT('Ctrl Pts',(19.2989881366047,-45.2815256556052,-1.8522784706461));
#7906=CARTESIAN_POINT('Ctrl Pts',(19.2955400517893,-45.290535759037,-1.86541441902233));
#7907=CARTESIAN_POINT('Ctrl Pts',(19.2872838742066,-45.3077809202632,-1.89168343393709));
#7908=CARTESIAN_POINT('Ctrl Pts',(19.2824758531213,-45.3160216986954,-1.90482330786193));
#7909=CARTESIAN_POINT('Ctrl Pts',(19.2714947564013,-45.3317383217991,-1.93111314012225));
#7910=CARTESIAN_POINT('Ctrl Pts',(19.2653276103518,-45.3392082270028,-1.94425196045163));
#7911=CARTESIAN_POINT('Ctrl Pts',(19.2515609423283,-45.3533830770125,-1.97058421507986));
#7912=CARTESIAN_POINT('Ctrl Pts',(19.244064213872,-45.3599773095852,-1.98357519226534));
#7913=CARTESIAN_POINT('Ctrl Pts',(19.2279384887284,-45.3721611568294,-2.00912118369974));
#7914=CARTESIAN_POINT('Ctrl Pts',(19.2192997653202,-45.37776054843,-2.02169452303134));
#7915=CARTESIAN_POINT('Ctrl Pts',(19.2008823814414,-45.3879779405028,-2.04643994358655));
#7916=CARTESIAN_POINT('Ctrl Pts',(19.1910930202263,-45.3925988298126,-2.05862275579914));
#7917=CARTESIAN_POINT('Ctrl Pts',(19.1703915953673,-45.4008287111318,-2.08254175691223));
#7918=CARTESIAN_POINT('Ctrl Pts',(19.1593769020686,-45.4044612308546,-2.09437589174056));
#7919=CARTESIAN_POINT('Ctrl Pts',(19.1365984286433,-45.4105559999369,-2.11715811641161));
#7920=CARTESIAN_POINT('Ctrl Pts',(19.1247946980441,-45.4130446424486,-2.12816493034605));
#7921=CARTESIAN_POINT('Ctrl Pts',(19.1003849579208,-45.4169112106896,-2.14940462118797));
#7922=CARTESIAN_POINT('Ctrl Pts',(19.0877771726989,-45.4182909661987,-2.15964088112869));
#7923=CARTESIAN_POINT('Ctrl Pts',(19.0617491248472,-45.4199293752183,-2.17933956376603));
#7924=CARTESIAN_POINT('Ctrl Pts',(19.0483317526372,-45.4201882850831,-2.1888003047611));
#7925=CARTESIAN_POINT('Ctrl Pts',(19.0206432686844,-45.4195375776723,-2.20692604496228));
#7926=CARTESIAN_POINT('Ctrl Pts',(19.0065974658149,-45.418632682757,-2.21544292771705));
#7927=CARTESIAN_POINT('Ctrl Pts',(18.9781346138199,-45.415695036091,-2.23140600796168));
#7928=CARTESIAN_POINT('Ctrl Pts',(18.9637143613756,-45.4136621054362,-2.23885416694541));
#7929=CARTESIAN_POINT('Ctrl Pts',(18.9344985968864,-45.4084658423515,-2.25268578324637));
#7930=CARTESIAN_POINT('Ctrl Pts',(18.9196997691129,-45.4053010066314,-2.25906973315595));
#7931=CARTESIAN_POINT('Ctrl Pts',(18.8972234079784,-45.399684523811,-2.26782447509019));
#7932=CARTESIAN_POINT('Ctrl Pts',(18.8896670993892,-45.3976611130282,-2.27061057640927));
#7933=CARTESIAN_POINT('Ctrl Pts',(18.8745247920546,-45.3933350465311,-2.27587916719238));
#7934=CARTESIAN_POINT('Ctrl Pts',(18.86697271241,-45.3910428501848,-2.27835075020622));
#7935=CARTESIAN_POINT('Ctrl Pts',(18.8443734352162,-45.3837824914105,-2.28528292905637));
#7936=CARTESIAN_POINT('Ctrl Pts',(18.8293452614729,-45.3784237192965,-2.28927880462709));
#7937=CARTESIAN_POINT('Ctrl Pts',(18.8143835621595,-45.3725581651887,-2.29264601963605));
#7938=CARTESIAN_POINT('Ctrl Pts',(18.6221620196843,-45.62059505756,-1.77871850124803));
#7939=CARTESIAN_POINT('Ctrl Pts',(18.6129193730699,-45.6172932558704,-1.78058192917525));
#7940=CARTESIAN_POINT('Ctrl Pts',(18.6037208544611,-45.6136589591554,-1.78208130646566));
#7941=CARTESIAN_POINT('Ctrl Pts',(18.5900102210826,-45.6077105512134,-1.78377425389336));
#7942=CARTESIAN_POINT('Ctrl Pts',(18.5854465361298,-45.6056405946596,-1.78424599704345));
#7943=CARTESIAN_POINT('Ctrl Pts',(18.576354527559,-45.6013345885701,-1.78500009038837));
#7944=CARTESIAN_POINT('Ctrl Pts',(18.5718108421278,-45.5990902159595,-1.78528264628693));
#7945=CARTESIAN_POINT('Ctrl Pts',(18.5583557915536,-45.592164749705,-1.78583455232009));
#7946=CARTESIAN_POINT('Ctrl Pts',(18.549597268328,-45.5872853986604,-1.78581522368785));
#7947=CARTESIAN_POINT('Ctrl Pts',(18.5324696592232,-45.5770009406535,-1.78502001129054));
#7948=CARTESIAN_POINT('Ctrl Pts',(18.5241044984817,-45.5715981948212,-1.7842443140869));
#7949=CARTESIAN_POINT('Ctrl Pts',(18.5077731763177,-45.560269424572,-1.78193347961354));
#7950=CARTESIAN_POINT('Ctrl Pts',(18.4998161446777,-45.554350730268,-1.78040065085215));
#7951=CARTESIAN_POINT('Ctrl Pts',(18.4881626129628,-45.5450449208074,-1.77750557246982));
#7952=CARTESIAN_POINT('Ctrl Pts',(18.4843505062967,-45.54189107573,-1.77644663525675));
#7953=CARTESIAN_POINT('Ctrl Pts',(18.4769071413954,-45.5355132808845,-1.77415492247898));
#7954=CARTESIAN_POINT('Ctrl Pts',(18.4732672288629,-45.5322824364064,-1.77292001334332));
#7955=CARTESIAN_POINT('Ctrl Pts',(18.4626004022307,-45.5224752605349,-1.7689552464585));
#7956=CARTESIAN_POINT('Ctrl Pts',(18.4558179103171,-45.5157781683263,-1.76596391369291));
#7957=CARTESIAN_POINT('Ctrl Pts',(18.4429084062604,-45.5020723540079,-1.75929249956289));
#7958=CARTESIAN_POINT('Ctrl Pts',(18.4367785698554,-45.4950591040281,-1.75560939899404));
#7959=CARTESIAN_POINT('Ctrl Pts',(18.4251947575442,-45.4807293651287,-1.74755147248085));
#7960=CARTESIAN_POINT('Ctrl Pts',(18.4197116844311,-45.4733619559223,-1.74314118482812));
#7961=CARTESIAN_POINT('Ctrl Pts',(18.4096841967476,-45.4586601759361,-1.73382309642942));
#7962=CARTESIAN_POINT('Ctrl Pts',(18.4050855722086,-45.4512635702888,-1.72888250720206));
#7963=CARTESIAN_POINT('Ctrl Pts',(18.3967294933308,-45.4364159601022,-1.71846981786302));
#7964=CARTESIAN_POINT('Ctrl Pts',(18.3929666633764,-45.4289582747971,-1.71299394688883));
#7965=CARTESIAN_POINT('Ctrl Pts',(18.387949845685,-45.4177241224448,-1.7043764995696));
#7966=CARTESIAN_POINT('Ctrl Pts',(18.3863815973451,-45.4139692966578,-1.70143483928496));
#7967=CARTESIAN_POINT('Ctrl Pts',(18.3834588294126,-45.4064475115089,-1.69541819155667));
#7968=CARTESIAN_POINT('Ctrl Pts',(18.3821013440093,-45.4026715013318,-1.69233565252243));
#7969=CARTESIAN_POINT('Ctrl Pts',(18.3783678140288,-45.3913602280059,-1.68291331926215));
#7970=CARTESIAN_POINT('Ctrl Pts',(18.3763571442371,-45.3839334687444,-1.67647740418325));
#7971=CARTESIAN_POINT('Ctrl Pts',(18.373239274455,-45.3692470015761,-1.66326464104222));
#7972=CARTESIAN_POINT('Ctrl Pts',(18.3721351020341,-45.361996292618,-1.65649525672691));
#7973=CARTESIAN_POINT('Ctrl Pts',(18.3708276406403,-45.3476781657535,-1.64263357999033));
#7974=CARTESIAN_POINT('Ctrl Pts',(18.3706250612,-45.3406095748083,-1.635539689768));
#7975=CARTESIAN_POINT('Ctrl Pts',(18.3710077529534,-45.3301503262564,-1.62465679749559));
#7976=CARTESIAN_POINT('Ctrl Pts',(18.3712517326172,-45.3266799167243,-1.62097960829253));
#7977=CARTESIAN_POINT('Ctrl Pts',(18.3719701704098,-45.3198204005466,-1.61357771003206));
#7978=CARTESIAN_POINT('Ctrl Pts',(18.3724424090973,-45.3164453844991,-1.60986862656259));
#7979=CARTESIAN_POINT('Ctrl Pts',(18.3741925883538,-45.3064826315517,-1.59871817096884));
#7980=CARTESIAN_POINT('Ctrl Pts',(18.3758024868939,-45.300037895571,-1.59123476923353));
#7981=CARTESIAN_POINT('Ctrl Pts',(18.3798873333543,-45.287560207475,-1.57619835335595));
#7982=CARTESIAN_POINT('Ctrl Pts',(18.3823625923558,-45.2815224282728,-1.56864024051346));
#7983=CARTESIAN_POINT('Ctrl Pts',(18.3881814606797,-45.2698526364099,-1.55344639789905));
#7984=CARTESIAN_POINT('Ctrl Pts',(18.3915297734654,-45.2642137421464,-1.54580098849944));
#7985=CARTESIAN_POINT('Ctrl Pts',(18.3991069351451,-45.2533791834234,-1.53046386154549));
#7986=CARTESIAN_POINT('Ctrl Pts',(18.4032741386649,-45.2482681928533,-1.52289338059093));
#7987=CARTESIAN_POINT('Ctrl Pts',(18.4123563475389,-45.2386112685697,-1.50790546647126));
#7988=CARTESIAN_POINT('Ctrl Pts',(18.4172683983267,-45.2340697519755,-1.50049420992322));
#7989=CARTESIAN_POINT('Ctrl Pts',(18.4278282750222,-45.2255558775991,-1.48583573393937));
#7990=CARTESIAN_POINT('Ctrl Pts',(18.4334801703118,-45.2215821677685,-1.47858483274337));
#7991=CARTESIAN_POINT('Ctrl Pts',(18.4455181297567,-45.2142206641317,-1.46426506544444));
#7992=CARTESIAN_POINT('Ctrl Pts',(18.4519528219293,-45.2108157610502,-1.45715123177322));
#7993=CARTESIAN_POINT('Ctrl Pts',(18.4652968721977,-45.2047449038404,-1.44340852007555));
#7994=CARTESIAN_POINT('Ctrl Pts',(18.4722504447086,-45.2020474267363,-1.43672247316454));
#7995=CARTESIAN_POINT('Ctrl Pts',(18.4866860257431,-45.1973329645429,-1.42374529115857));
#7996=CARTESIAN_POINT('Ctrl Pts',(18.4941721105413,-45.1953130577611,-1.41744886968267));
#7997=CARTESIAN_POINT('Ctrl Pts',(18.5096858061187,-45.1919542156582,-1.40524401960937));
#7998=CARTESIAN_POINT('Ctrl Pts',(18.5177148817011,-45.1906149853657,-1.39933446124003));
#7999=CARTESIAN_POINT('Ctrl Pts',(18.5343294229057,-45.1886445172451,-1.38792248147468));
#8000=CARTESIAN_POINT('Ctrl Pts',(18.542779440216,-45.188029106266,-1.38251285316967));
#8001=CARTESIAN_POINT('Ctrl Pts',(18.5599645231716,-45.1875150185148,-1.37226320603098));
#8002=CARTESIAN_POINT('Ctrl Pts',(18.5686982527055,-45.1876165784289,-1.36742418470241));
#8003=CARTESIAN_POINT('Ctrl Pts',(18.5864477638643,-45.1885360827692,-1.35831709053276));
#8004=CARTESIAN_POINT('Ctrl Pts',(18.5954684722606,-45.1893552624518,-1.35404748924571));
#8005=CARTESIAN_POINT('Ctrl Pts',(18.6137800334896,-45.1917248752601,-1.34610113724339));
#8006=CARTESIAN_POINT('Ctrl Pts',(18.6231272825575,-45.1932895780203,-1.34240702291553));
#8007=CARTESIAN_POINT('Ctrl Pts',(18.6417841046389,-45.1971209486494,-1.33575597841215));
#8008=CARTESIAN_POINT('Ctrl Pts',(18.6511507406784,-45.1993932961657,-1.33277254722322));
#8009=CARTESIAN_POINT('Ctrl Pts',(18.6699132468501,-45.204646120538,-1.32751128947911));
#8010=CARTESIAN_POINT('Ctrl Pts',(18.6793578875184,-45.207646105241,-1.32522575676464));
#8011=CARTESIAN_POINT('Ctrl Pts',(18.6979513544394,-45.214255255135,-1.32144333958208));
#8012=CARTESIAN_POINT('Ctrl Pts',(18.7071641468385,-45.2178802413143,-1.31992638960479));
#8013=CARTESIAN_POINT('Ctrl Pts',(18.7253869486455,-45.225754682879,-1.31764408095801));
#8014=CARTESIAN_POINT('Ctrl Pts',(18.7344068621661,-45.2300078746987,-1.316876927761));
#8015=CARTESIAN_POINT('Ctrl Pts',(18.7477801983432,-45.2368600692891,-1.31629654325037));
#8016=CARTESIAN_POINT('Ctrl Pts',(18.752219283311,-45.2392274939513,-1.31619867106209));
#8017=CARTESIAN_POINT('Ctrl Pts',(18.7610367701067,-45.2441187387261,-1.31619676023362));
#8018=CARTESIAN_POINT('Ctrl Pts',(18.7654325107433,-45.2466532619187,-1.3162938241929));
#8019=CARTESIAN_POINT('Ctrl Pts',(18.7784191500246,-45.2544329831877,-1.31687816890436));
#8020=CARTESIAN_POINT('Ctrl Pts',(18.7868169502624,-45.2598527540315,-1.31765275683562));
#8021=CARTESIAN_POINT('Ctrl Pts',(18.8031371766128,-45.2711680622823,-1.31995614213438));
#8022=CARTESIAN_POINT('Ctrl Pts',(18.8110542369534,-45.2770600838242,-1.3214843906258));
#8023=CARTESIAN_POINT('Ctrl Pts',(18.8264003541456,-45.2893146918086,-1.32529693961078));
#8024=CARTESIAN_POINT('Ctrl Pts',(18.8338206659933,-45.2956692062439,-1.32757795725868));
#8025=CARTESIAN_POINT('Ctrl Pts',(18.8445991939612,-45.3055898547247,-1.33159522925254));
#8026=CARTESIAN_POINT('Ctrl Pts',(18.8481102922723,-45.308941341363,-1.3330260675456));
#8027=CARTESIAN_POINT('Ctrl Pts',(18.8549328043703,-45.3156945009062,-1.33605192943852));
#8028=CARTESIAN_POINT('Ctrl Pts',(18.8582530677542,-45.3191042958294,-1.33765022769154));
#8029=CARTESIAN_POINT('Ctrl Pts',(18.867933585062,-45.3294204870494,-1.34269225948157));
#8030=CARTESIAN_POINT('Ctrl Pts',(18.8740225584048,-45.336421260905,-1.34638576214841));
#8031=CARTESIAN_POINT('Ctrl Pts',(18.8854757967299,-45.3506622005078,-1.35442702575445));
#8032=CARTESIAN_POINT('Ctrl Pts',(18.8908432353629,-45.3579082824918,-1.35877902402508));
#8033=CARTESIAN_POINT('Ctrl Pts',(18.9008330792294,-45.3726243827529,-1.36813301959756));
#8034=CARTESIAN_POINT('Ctrl Pts',(18.9054840795676,-45.380154146016,-1.37317976216689));
#8035=CARTESIAN_POINT('Ctrl Pts',(18.9138227526446,-45.3951016039498,-1.38370412631569));
#8036=CARTESIAN_POINT('Ctrl Pts',(18.9175551433971,-45.4025783442055,-1.38921665563984));
#8037=CARTESIAN_POINT('Ctrl Pts',(18.9241472981129,-45.4175069410417,-1.40071017489184));
#8038=CARTESIAN_POINT('Ctrl Pts',(18.9270110154327,-45.4249640522584,-1.40669428620247));
#8039=CARTESIAN_POINT('Ctrl Pts',(18.9318734081378,-45.4398636906155,-1.41913718051563));
#8040=CARTESIAN_POINT('Ctrl Pts',(18.9338726776514,-45.4473086206934,-1.42559807779935));
#8041=CARTESIAN_POINT('Ctrl Pts',(18.9369783416384,-45.4621742438128,-1.4390004513004));
#8042=CARTESIAN_POINT('Ctrl Pts',(18.9380587854086,-45.4694678481601,-1.44582700875946));
#8043=CARTESIAN_POINT('Ctrl Pts',(18.9393173410065,-45.4838003767252,-1.45973104908589));
#8044=CARTESIAN_POINT('Ctrl Pts',(18.9394948496878,-45.4908371992824,-1.46680673001694));
#8045=CARTESIAN_POINT('Ctrl Pts',(18.9389586363646,-45.504655487356,-1.4812020445518));
#8046=CARTESIAN_POINT('Ctrl Pts',(18.9382429617193,-45.5114415845077,-1.48852750652597));
#8047=CARTESIAN_POINT('Ctrl Pts',(18.935914549752,-45.5247359862846,-1.5034028039268));
#8048=CARTESIAN_POINT('Ctrl Pts',(18.9342813020382,-45.5312939444273,-1.51101488314489));
#8049=CARTESIAN_POINT('Ctrl Pts',(18.9301711295785,-45.543861814362,-1.52615759875804));
#8050=CARTESIAN_POINT('Ctrl Pts',(18.9276914024776,-45.5499184342165,-1.53373745384419));
#8051=CARTESIAN_POINT('Ctrl Pts',(18.9219044584414,-45.5615659591846,-1.5488905221349));
#8052=CARTESIAN_POINT('Ctrl Pts',(18.9185970863043,-45.5671606360396,-1.55646766958521));
#8053=CARTESIAN_POINT('Ctrl Pts',(18.9111518540018,-45.5778903308794,-1.5716231951062));
#8054=CARTESIAN_POINT('Ctrl Pts',(18.9070179238834,-45.5830212371186,-1.57919515593537));
#8055=CARTESIAN_POINT('Ctrl Pts',(18.8978775137544,-45.5928252580521,-1.59436601615716));
#8056=CARTESIAN_POINT('Ctrl Pts',(18.8929394538017,-45.5974219543871,-1.60184826399308));
#8057=CARTESIAN_POINT('Ctrl Pts',(18.8823875119263,-45.6059897116602,-1.61655719916668));
#8058=CARTESIAN_POINT('Ctrl Pts',(18.8767671790069,-45.6099675442075,-1.62379444292518));
#8059=CARTESIAN_POINT('Ctrl Pts',(18.8648446796018,-45.6173136869872,-1.63803320411293));
#8060=CARTESIAN_POINT('Ctrl Pts',(18.8585356910874,-45.620684256901,-1.645040886683));
#8061=CARTESIAN_POINT('Ctrl Pts',(18.8452471260023,-45.6267961002234,-1.65879399575824));
#8062=CARTESIAN_POINT('Ctrl Pts',(18.8382022586574,-45.629556299998,-1.66559567268411));
#8063=CARTESIAN_POINT('Ctrl Pts',(18.8236812226873,-45.6343318803847,-1.67868354354709));
#8064=CARTESIAN_POINT('Ctrl Pts',(18.816179049323,-45.6363659793353,-1.68500354300762));
#8065=CARTESIAN_POINT('Ctrl Pts',(18.8007069179842,-45.6397318406192,-1.69719202919393));
#8066=CARTESIAN_POINT('Ctrl Pts',(18.7927357842832,-45.6410648637206,-1.70306246701553));
#8067=CARTESIAN_POINT('Ctrl Pts',(18.7763184849427,-45.6430238072,-1.7143510708677));
#8068=CARTESIAN_POINT('Ctrl Pts',(18.7678741313109,-45.643649793127,-1.7197682782934));
#8069=CARTESIAN_POINT('Ctrl Pts',(18.750484658679,-45.6441668837513,-1.73013665595371));
#8070=CARTESIAN_POINT('Ctrl Pts',(18.7416810490484,-45.6440534227969,-1.7350030871688));
#8071=CARTESIAN_POINT('Ctrl Pts',(18.7238738472453,-45.6431037361945,-1.74411204981961));
#8072=CARTESIAN_POINT('Ctrl Pts',(18.7148682493225,-45.6422674984819,-1.74835570404536));
#8073=CARTESIAN_POINT('Ctrl Pts',(18.6966533086483,-45.6398726569234,-1.75622164832084));
#8074=CARTESIAN_POINT('Ctrl Pts',(18.6874419268025,-45.6383131841139,-1.75984420616735));
#8075=CARTESIAN_POINT('Ctrl Pts',(18.6734737700129,-45.6354195819173,-1.76479817562067));
#8076=CARTESIAN_POINT('Ctrl Pts',(18.6687815047508,-45.6343591081953,-1.76637215337371));
#8077=CARTESIAN_POINT('Ctrl Pts',(18.6593857582353,-45.6320583062489,-1.76934304099513));
#8078=CARTESIAN_POINT('Ctrl Pts',(18.6547033024031,-45.6308236309591,-1.77073381700843));
#8079=CARTESIAN_POINT('Ctrl Pts',(18.6407016991349,-45.6268695302727,-1.77462522039306));
#8080=CARTESIAN_POINT('Ctrl Pts',(18.6314046662986,-45.6238968592495,-1.77685507332082));
#8081=CARTESIAN_POINT('Ctrl Pts',(18.6221620196843,-45.62059505756,-1.77871850124803));
#8082=CARTESIAN_POINT('Ctrl Pts',(18.8143835720322,-45.3725581690592,-2.29264601741413));
#8083=CARTESIAN_POINT('Ctrl Pts',(18.8004239876014,-45.3670854822463,-2.29578770105548));
#8084=CARTESIAN_POINT('Ctrl Pts',(18.7868223091714,-45.3612925527447,-2.29831830851143));
#8085=CARTESIAN_POINT('Ctrl Pts',(18.7734632629,-45.3551737210001,-2.30031107484356));
#8086=CARTESIAN_POINT('Ctrl Pts',(18.7721970853537,-45.3545937748568,-2.30049995030169));
#8087=CARTESIAN_POINT('Ctrl Pts',(18.7709330877609,-45.3540108759632,-2.30068396486783));
#8088=CARTESIAN_POINT('Ctrl Pts',(18.7696711723614,-45.3534250039398,-2.30086316260009));
#8089=CARTESIAN_POINT('Ctrl Pts',(18.7622047899902,-45.3499585714448,-2.30192342289145));
#8090=CARTESIAN_POINT('Ctrl Pts',(18.7547981841974,-45.346380911665,-2.30281570621072));
#8091=CARTESIAN_POINT('Ctrl Pts',(18.747446675797,-45.3426929858494,-2.30354453863187));
#8092=CARTESIAN_POINT('Ctrl Pts',(18.7400309651229,-45.3389728525998,-2.30427973610029));
#8093=CARTESIAN_POINT('Ctrl Pts',(18.7326462625095,-45.3351263544063,-2.30484927334382));
#8094=CARTESIAN_POINT('Ctrl Pts',(18.7253607974182,-45.3311904062177,-2.30524970736628));
#8095=CARTESIAN_POINT('Ctrl Pts',(18.7123145848033,-45.3241422334153,-2.3059667717307));
#8096=CARTESIAN_POINT('Ctrl Pts',(18.6995547694162,-45.3167993788134,-2.3061540494447));
#8097=CARTESIAN_POINT('Ctrl Pts',(18.6869391162223,-45.3090816154315,-2.30581663077418));
#8098=CARTESIAN_POINT('Ctrl Pts',(18.6854534455579,-45.3081727402051,-2.30577689497828));
#8099=CARTESIAN_POINT('Ctrl Pts',(18.6839697956892,-45.3072586368875,-2.30572983528853));
#8100=CARTESIAN_POINT('Ctrl Pts',(18.6824879511072,-45.3063391513267,-2.30567542238217));
#8101=CARTESIAN_POINT('Ctrl Pts',(18.6722737305609,-45.3000012206008,-2.3053003591449));
#8102=CARTESIAN_POINT('Ctrl Pts',(18.6621479860631,-45.2934106165849,-2.30457758487901));
#8103=CARTESIAN_POINT('Ctrl Pts',(18.6520560907276,-45.286510756581,-2.30347965695592));
#8104=CARTESIAN_POINT('Ctrl Pts',(18.6484920955429,-45.2840740420678,-2.30309191910282));
#8105=CARTESIAN_POINT('Ctrl Pts',(18.6449539352567,-45.2816133646422,-2.30265953234694));
#8106=CARTESIAN_POINT('Ctrl Pts',(18.6414409530944,-45.2791285251635,-2.30218272861357));
#8107=CARTESIAN_POINT('Ctrl Pts',(18.628011060722,-45.2696291524881,-2.30035994030265));
#8108=CARTESIAN_POINT('Ctrl Pts',(18.6149637231189,-45.2597892538428,-2.29789258754658));
#8109=CARTESIAN_POINT('Ctrl Pts',(18.6022294924165,-45.2495457329913,-2.29475584752329));
#8110=CARTESIAN_POINT('Ctrl Pts',(18.5958359434542,-45.2444027091494,-2.29318096629256));
#8111=CARTESIAN_POINT('Ctrl Pts',(18.589563243215,-45.2391901429808,-2.29144593577685));
#8112=CARTESIAN_POINT('Ctrl Pts',(18.5834369872997,-45.2339331804978,-2.28956226538368));
#8113=CARTESIAN_POINT('Ctrl Pts',(18.5773027399217,-45.2286693605116,-2.28767613781572));
#8114=CARTESIAN_POINT('Ctrl Pts',(18.5713010530664,-45.2233495740206,-2.28563749245308));
#8115=CARTESIAN_POINT('Ctrl Pts',(18.5654325544997,-45.2179770224707,-2.28344953823052));
#8116=CARTESIAN_POINT('Ctrl Pts',(18.553698651473,-45.2072347519946,-2.27907478336218));
#8117=CARTESIAN_POINT('Ctrl Pts',(18.542482749313,-45.1962715684224,-2.27410148247452));
#8118=CARTESIAN_POINT('Ctrl Pts',(18.5317611930651,-45.185066998578,-2.26852163941299));
#8119=CARTESIAN_POINT('Ctrl Pts',(18.5265356102954,-45.1796059996551,-2.26580207789727));
#8120=CARTESIAN_POINT('Ctrl Pts',(18.5214264579813,-45.1740858650027,-2.26293705907253));
#8121=CARTESIAN_POINT('Ctrl Pts',(18.5164344168917,-45.1685050515947,-2.2599242470794));
#8122=CARTESIAN_POINT('Ctrl Pts',(18.5112098007234,-45.1626642326909,-2.25677107065937));
#8123=CARTESIAN_POINT('Ctrl Pts',(18.5061284176769,-45.1567736219033,-2.25346498673654));
#8124=CARTESIAN_POINT('Ctrl Pts',(18.5011909625963,-45.1508342975478,-2.25000661864255));
#8125=CARTESIAN_POINT('Ctrl Pts',(18.491508410506,-45.1391870386839,-2.24322461684791));
#8126=CARTESIAN_POINT('Ctrl Pts',(18.4823299625097,-45.1272711143548,-2.23579736542041));
#8127=CARTESIAN_POINT('Ctrl Pts',(18.4739101995274,-45.1154323141895,-2.22794676536405));
#8128=CARTESIAN_POINT('Ctrl Pts',(18.4654702471985,-45.103565126332,-2.2200773407296));
#8129=CARTESIAN_POINT('Ctrl Pts',(18.4577018487684,-45.091673400839,-2.21172713083511));
#8130=CARTESIAN_POINT('Ctrl Pts',(18.4506043254293,-45.0797770058834,-2.20291734912335));
#8131=CARTESIAN_POINT('Ctrl Pts',(18.4435022248184,-45.0678729388103,-2.19410188588521));
#8132=CARTESIAN_POINT('Ctrl Pts',(18.4370628910371,-45.0559533293678,-2.18481990262873));
#8133=CARTESIAN_POINT('Ctrl Pts',(18.4312854178286,-45.0440123208978,-2.17506295044399));
#8134=CARTESIAN_POINT('Ctrl Pts',(18.4283984600337,-45.0380454931449,-2.17018747839114));
#8135=CARTESIAN_POINT('Ctrl Pts',(18.4256758338712,-45.0320698970282,-2.1651901129344));
#8136=CARTESIAN_POINT('Ctrl Pts',(18.4231219961346,-45.0260908918466,-2.16007363253705));
#8137=CARTESIAN_POINT('Ctrl Pts',(18.4205706988703,-45.0201178343793,-2.15496224184333));
#8138=CARTESIAN_POINT('Ctrl Pts',(18.418182587299,-45.0141270383902,-2.14971911935779));
#8139=CARTESIAN_POINT('Ctrl Pts',(18.4159733552971,-45.0081503497711,-2.14436973787106));
#8140=CARTESIAN_POINT('Ctrl Pts',(18.4115653077667,-44.9962251524691,-2.13369619709656));
#8141=CARTESIAN_POINT('Ctrl Pts',(18.4079166371414,-44.9845006989954,-2.12273326060535));
#8142=CARTESIAN_POINT('Ctrl Pts',(18.4049873524301,-44.9729204300536,-2.11144045659183));
#8143=CARTESIAN_POINT('Ctrl Pts',(18.4020714181278,-44.9613929389545,-2.1001991202805));
#8144=CARTESIAN_POINT('Ctrl Pts',(18.3998736076026,-44.9500224126483,-2.08864349710599));
#8145=CARTESIAN_POINT('Ctrl Pts',(18.3983959092214,-44.9388017294662,-2.07676095428626));
#8146=CARTESIAN_POINT('Ctrl Pts',(18.3969534133881,-44.9278483516032,-2.06516148397203));
#8147=CARTESIAN_POINT('Ctrl Pts',(18.3961981046829,-44.9170360420461,-2.05324784150275));
#8148=CARTESIAN_POINT('Ctrl Pts',(18.3961530998036,-44.9063694860149,-2.04100636176672));
#8149=CARTESIAN_POINT('Ctrl Pts',(18.3961522869288,-44.9061768274623,-2.04078525705771));
#8150=CARTESIAN_POINT('Ctrl Pts',(18.3961517065425,-44.9059843646424,-2.04056421547236));
#8151=CARTESIAN_POINT('Ctrl Pts',(18.3961513577277,-44.9057920947054,-2.040343234352));
#8152=CARTESIAN_POINT('Ctrl Pts',(18.3961413899904,-44.9002977855887,-2.03402847395322));
#8153=CARTESIAN_POINT('Ctrl Pts',(18.3963218076041,-44.8949486379762,-2.02774797606833));
#8154=CARTESIAN_POINT('Ctrl Pts',(18.3966783095951,-44.8897170364107,-2.02147951930314));
#8155=CARTESIAN_POINT('Ctrl Pts',(18.3970409778534,-44.8843949459994,-2.01510263963699));
#8156=CARTESIAN_POINT('Ctrl Pts',(18.3975832129578,-44.879215584956,-2.00876434096866));
#8157=CARTESIAN_POINT('Ctrl Pts',(18.3983054323315,-44.8741136640234,-2.00238878355093));
#8158=CARTESIAN_POINT('Ctrl Pts',(18.3992264158328,-44.867607628357,-1.99425859013933));
#8159=CARTESIAN_POINT('Ctrl Pts',(18.4004372205309,-44.861214582528,-1.98605493790166));
#8160=CARTESIAN_POINT('Ctrl Pts',(18.4019814199691,-44.8548256801295,-1.97762112291159));
#8161=CARTESIAN_POINT('Ctrl Pts',(18.4024376090313,-44.8529382636973,-1.97512959619772));
#8162=CARTESIAN_POINT('Ctrl Pts',(18.4029231971869,-44.8510513677406,-1.97261795136468));
#8163=CARTESIAN_POINT('Ctrl Pts',(18.403440078478,-44.8491626004708,-1.97008207935643));
#8164=CARTESIAN_POINT('Ctrl Pts',(18.4038588959962,-44.8476321739806,-1.96802731815887));
#8165=CARTESIAN_POINT('Ctrl Pts',(18.4043018647573,-44.8460878557025,-1.96593952534612));
#8166=CARTESIAN_POINT('Ctrl Pts',(18.4047663150324,-44.8445433944683,-1.96383639013916));
#8167=CARTESIAN_POINT('Ctrl Pts',(18.4059382132851,-44.8406464187982,-1.9585297715262));
#8168=CARTESIAN_POINT('Ctrl Pts',(18.4072504491973,-44.836749090789,-1.95312358986634));
#8169=CARTESIAN_POINT('Ctrl Pts',(18.4086264109651,-44.8330535376181,-1.94790428743763));
#8170=CARTESIAN_POINT('Ctrl Pts',(18.409982715073,-44.8294107809196,-1.94275955050535));
#8171=CARTESIAN_POINT('Ctrl Pts',(18.4114002396028,-44.825963730331,-1.93779647790292));
#8172=CARTESIAN_POINT('Ctrl Pts',(18.4127613885304,-44.8228831621709,-1.93329453562058));
#8173=CARTESIAN_POINT('Ctrl Pts',(18.4136001434265,-44.8209848822878,-1.9305203894159));
#8174=CARTESIAN_POINT('Ctrl Pts',(18.414487376004,-44.8190644191933,-1.92768639394373));
#8175=CARTESIAN_POINT('Ctrl Pts',(18.4154262847733,-44.8171251875568,-1.92479418624063));
#8176=CARTESIAN_POINT('Ctrl Pts',(18.4181694429729,-44.8114594409591,-1.916344181793));
#8177=CARTESIAN_POINT('Ctrl Pts',(18.4213570016482,-44.8056288168499,-1.90738961609199));
#8178=CARTESIAN_POINT('Ctrl Pts',(18.425067403476,-44.7997293148395,-1.89798447547152));
#8179=CARTESIAN_POINT('Ctrl Pts',(18.4267071356894,-44.7971221569254,-1.89382807604023));
#8180=CARTESIAN_POINT('Ctrl Pts',(18.4284458771357,-44.7945059656841,-1.88959094729095));
#8181=CARTESIAN_POINT('Ctrl Pts',(18.4302982493404,-44.7918774552728,-1.88525884485412));
#8182=CARTESIAN_POINT('Ctrl Pts',(18.4312589896668,-44.7905141677304,-1.88301198242625));
#8183=CARTESIAN_POINT('Ctrl Pts',(18.4322476807013,-44.7891512009799,-1.88074559978552));
#8184=CARTESIAN_POINT('Ctrl Pts',(18.4332663774496,-44.7877881173523,-1.87845772299634));
#8185=CARTESIAN_POINT('Ctrl Pts',(18.43459451111,-44.7860109866696,-1.87547488617116));
#8186=CARTESIAN_POINT('Ctrl Pts',(18.4360905916004,-44.7840843386202,-1.87220096972747));
#8187=CARTESIAN_POINT('Ctrl Pts',(18.437552740056,-44.7822772399823,-1.86908824391098));
#8188=CARTESIAN_POINT('Ctrl Pts',(18.4391864896795,-44.780258056015,-1.86561020130088));
#8189=CARTESIAN_POINT('Ctrl Pts',(18.4407777072385,-44.7783878950342,-1.86233324968192));
#8190=CARTESIAN_POINT('Ctrl Pts',(18.4419912296012,-44.7769984935751,-1.85987648243287));
#8191=CARTESIAN_POINT('Ctrl Pts',(18.4421307944011,-44.7768387012692,-1.85959393450455));
#8192=CARTESIAN_POINT('Ctrl Pts',(18.4422653209045,-44.7766852340587,-1.85932222665245));
#8193=CARTESIAN_POINT('Ctrl Pts',(18.4423942727962,-44.7765385757179,-1.85906229563845));
#8194=CARTESIAN_POINT('Ctrl Pts',(18.4442993095736,-44.7743719573813,-1.85522227332556));
#8195=CARTESIAN_POINT('Ctrl Pts',(18.4464978127059,-44.7719689214077,-1.85090212076217));
#8196=CARTESIAN_POINT('Ctrl Pts',(18.4491297065906,-44.7692782255981,-1.84594334195215));
#8197=CARTESIAN_POINT('Ctrl Pts',(18.4515807522943,-44.7667724184899,-1.84132530109245));
#8198=CARTESIAN_POINT('Ctrl Pts',(18.4544067332379,-44.7640174757803,-1.83615446044127));
#8199=CARTESIAN_POINT('Ctrl Pts',(18.4577529093881,-44.7609994330517,-1.83031111945421));
#8200=CARTESIAN_POINT('Ctrl Pts',(18.4593149008355,-44.7595906139345,-1.82758345413227));
#8201=CARTESIAN_POINT('Ctrl Pts',(18.4609907570087,-44.7581248818874,-1.82470935927919));
#8202=CARTESIAN_POINT('Ctrl Pts',(18.4627983272808,-44.7566033146199,-1.8216773121477));
#8203=CARTESIAN_POINT('Ctrl Pts',(18.465907725695,-44.7539859011107,-1.81646155777946));
#8204=CARTESIAN_POINT('Ctrl Pts',(18.468851062055,-44.7516706279046,-1.81171012416722));
#8205=CARTESIAN_POINT('Ctrl Pts',(18.4715899190303,-44.7496144243376,-1.80740112264175));
#8206=CARTESIAN_POINT('Ctrl Pts',(18.4755934405833,-44.7466087707485,-1.80110244380068));
#8207=CARTESIAN_POINT('Ctrl Pts',(18.4791597997392,-44.7441550963149,-1.79574749180543));
#8208=CARTESIAN_POINT('Ctrl Pts',(18.4822053765618,-44.7421501763609,-1.79127796352151));
#8209=CARTESIAN_POINT('Ctrl Pts',(18.4836683130458,-44.7411871172364,-1.78913103491851));
#8210=CARTESIAN_POINT('Ctrl Pts',(18.4850117290154,-44.7403280695135,-1.78718848257471));
#8211=CARTESIAN_POINT('Ctrl Pts',(18.486229714533,-44.7395641131514,-1.78544433398189));
#8212=CARTESIAN_POINT('Ctrl Pts',(18.4873872880559,-44.7388380489704,-1.78378669503485));
#8213=CARTESIAN_POINT('Ctrl Pts',(18.4891933860945,-44.7377225025067,-1.78121987593171));
#8214=CARTESIAN_POINT('Ctrl Pts',(18.4912772121235,-44.736491572082,-1.77832245138861));
#8215=CARTESIAN_POINT('Ctrl Pts',(18.4932650638731,-44.7353173343269,-1.7755584728382));
#8216=CARTESIAN_POINT('Ctrl Pts',(18.4955070564238,-44.7340392999125,-1.77249400980688));
#8217=CARTESIAN_POINT('Ctrl Pts',(18.4976460311451,-44.73286651034,-1.7696234929949));
#8218=CARTESIAN_POINT('Ctrl Pts',(18.498580264236,-44.7323542748206,-1.76836974662419));
#8219=CARTESIAN_POINT('Ctrl Pts',(18.4994950361885,-44.7318614215613,-1.76715206750054));
#8220=CARTESIAN_POINT('Ctrl Pts',(18.5003576343236,-44.7314034029234,-1.76601151907465));
#8221=CARTESIAN_POINT('Ctrl Pts',(18.5052655100644,-44.7287974402272,-1.75952220531098));
#8222=CARTESIAN_POINT('Ctrl Pts',(18.5101114448029,-44.7264480717817,-1.75337123329988));
#8223=CARTESIAN_POINT('Ctrl Pts',(18.5148610415796,-44.7243168044746,-1.74753823326662));
#8224=CARTESIAN_POINT('Ctrl Pts',(18.5190637936833,-44.7224309205608,-1.74237681550574));
#8225=CARTESIAN_POINT('Ctrl Pts',(18.5231989650652,-44.7207126167444,-1.73745616497633));
#8226=CARTESIAN_POINT('Ctrl Pts',(18.5272331822637,-44.7191479490509,-1.73278354382904));
#8227=CARTESIAN_POINT('Ctrl Pts',(18.5323172306827,-44.7171761052155,-1.72689495851323));
#8228=CARTESIAN_POINT('Ctrl Pts',(18.5372581723168,-44.7154369208339,-1.72137500930987));
#8229=CARTESIAN_POINT('Ctrl Pts',(18.542026435158,-44.7138915816973,-1.71619922278658));
#8230=CARTESIAN_POINT('Ctrl Pts',(18.5452525177388,-44.7128460454431,-1.71269742028524));
#8231=CARTESIAN_POINT('Ctrl Pts',(18.5490365918176,-44.7116862681572,-1.70866569029123));
#8232=CARTESIAN_POINT('Ctrl Pts',(18.5531138200782,-44.7105402951052,-1.70443999061808));
#8233=CARTESIAN_POINT('Ctrl Pts',(18.5552257322364,-44.7099467069452,-1.70225117362124));
#8234=CARTESIAN_POINT('Ctrl Pts',(18.5574158606756,-44.7093563068657,-1.70001003806637));
#8235=CARTESIAN_POINT('Ctrl Pts',(18.5596440490768,-44.708782795066,-1.69776098915752));
#8236=CARTESIAN_POINT('Ctrl Pts',(18.5637477023021,-44.7077265587329,-1.69361891714801));
#8237=CARTESIAN_POINT('Ctrl Pts',(18.5679830742223,-44.706729306282,-1.68945007474751));
#8238=CARTESIAN_POINT('Ctrl Pts',(18.5720778157018,-44.7058476668227,-1.68551414114025));
#8239=CARTESIAN_POINT('Ctrl Pts',(18.5728458353102,-44.7056823043949,-1.68477590792015));
#8240=CARTESIAN_POINT('Ctrl Pts',(18.5736088231611,-44.7055209032599,-1.68404580744789));
#8241=CARTESIAN_POINT('Ctrl Pts',(18.5743648681294,-44.7053636940034,-1.68332547089644));
#8242=CARTESIAN_POINT('Ctrl Pts',(18.58122353312,-44.7039375280099,-1.67679074439966));
#8243=CARTESIAN_POINT('Ctrl Pts',(18.5880173171863,-44.7027501655137,-1.67057651486332));
#8244=CARTESIAN_POINT('Ctrl Pts',(18.5947210176705,-44.7017664392736,-1.66466019129503));
#8245=CARTESIAN_POINT('Ctrl Pts',(18.5989653103428,-44.7011436157925,-1.66091440807775));
#8246=CARTESIAN_POINT('Ctrl Pts',(18.6031738180247,-44.7006024502006,-1.65728783989602));
#8247=CARTESIAN_POINT('Ctrl Pts',(18.6073407582855,-44.700135176751,-1.65377565492483));
#8248=CARTESIAN_POINT('Ctrl Pts',(18.6125018364014,-44.6995564224076,-1.64942554192594));
#8249=CARTESIAN_POINT('Ctrl Pts',(18.6181386121197,-44.6990337803828,-1.64479966015728));
#8250=CARTESIAN_POINT('Ctrl Pts',(18.6240306101813,-44.6986245769102,-1.64012155899839));
#8251=CARTESIAN_POINT('Ctrl Pts',(18.6268033999718,-44.6984320046794,-1.63792003228428));
#8252=CARTESIAN_POINT('Ctrl Pts',(18.6296323111388,-44.6982640568705,-1.63570665739715));
#8253=CARTESIAN_POINT('Ctrl Pts',(18.6324920213832,-44.6981237807725,-1.63350305160767));
#8254=CARTESIAN_POINT('Ctrl Pts',(18.6362109497917,-44.6979413578269,-1.63063735841798));
#8255=CARTESIAN_POINT('Ctrl Pts',(18.6399646635497,-44.6978067642329,-1.62780173184111));
#8256=CARTESIAN_POINT('Ctrl Pts',(18.6436937629378,-44.697720531018,-1.62503928727001));
#8257=CARTESIAN_POINT('Ctrl Pts',(18.6519075484317,-44.6975305920927,-1.61895467412767));
#8258=CARTESIAN_POINT('Ctrl Pts',(18.6599702366363,-44.697569880747,-1.61324230583385));
#8259=CARTESIAN_POINT('Ctrl Pts',(18.6680416881922,-44.6978090218053,-1.60775448089976));
#8260=CARTESIAN_POINT('Ctrl Pts',(18.6694848509728,-44.6978517798486,-1.60677326647549));
#8261=CARTESIAN_POINT('Ctrl Pts',(18.6709283344754,-44.697901024391,-1.60579931342513));
#8262=CARTESIAN_POINT('Ctrl Pts',(18.6723731047756,-44.6979567121928,-1.60483188349929));
#8263=CARTESIAN_POINT('Ctrl Pts',(18.6805679321806,-44.6982725768841,-1.59934456051963));
#8264=CARTESIAN_POINT('Ctrl Pts',(18.6888021087005,-44.6987928324897,-1.59406520294023));
#8265=CARTESIAN_POINT('Ctrl Pts',(18.6972615123352,-44.6995351544724,-1.5888818875588));
#8266=CARTESIAN_POINT('Ctrl Pts',(18.7026429287197,-44.7000073796851,-1.58558454184454));
#8267=CARTESIAN_POINT('Ctrl Pts',(18.7081158005212,-44.7005701960318,-1.58232667770584));
#8268=CARTESIAN_POINT('Ctrl Pts',(18.7137314098992,-44.7012361070428,-1.57908626479971));
#8269=CARTESIAN_POINT('Ctrl Pts',(18.7159232409764,-44.7014960190755,-1.57782149774905));
#8270=CARTESIAN_POINT('Ctrl Pts',(18.7181370386302,-44.7017717646743,-1.57655937941308));
#8271=CARTESIAN_POINT('Ctrl Pts',(18.7203759135888,-44.7020643954889,-1.57529891730949));
#8272=CARTESIAN_POINT('Ctrl Pts',(18.7326429648932,-44.7036677531046,-1.56839270165288));
#8273=CARTESIAN_POINT('Ctrl Pts',(18.7447343611095,-44.7056570974029,-1.56206039186384));
#8274=CARTESIAN_POINT('Ctrl Pts',(18.7565711408401,-44.7079508087299,-1.55626683595386));
#8275=CARTESIAN_POINT('Ctrl Pts',(18.7579890031085,-44.7082255597026,-1.55557285798758));
#8276=CARTESIAN_POINT('Ctrl Pts',(18.7594040701221,-44.7085049379473,-1.55488629909964));
#8277=CARTESIAN_POINT('Ctrl Pts',(18.7608158989421,-44.7087887219445,-1.55420722350708));
#8278=CARTESIAN_POINT('Ctrl Pts',(18.7674150186135,-44.7101151749334,-1.55103311271009));
#8279=CARTESIAN_POINT('Ctrl Pts',(18.7739379815234,-44.7115363266361,-1.54802478285648));
#8280=CARTESIAN_POINT('Ctrl Pts',(18.7803771570996,-44.713039660849,-1.54517187036228));
#8281=CARTESIAN_POINT('Ctrl Pts',(18.7819869509937,-44.7134154944022,-1.54445864223873));
#8282=CARTESIAN_POINT('Ctrl Pts',(18.7834188829847,-44.7137558360497,-1.54383126623162));
#8283=CARTESIAN_POINT('Ctrl Pts',(18.7847866301017,-44.7140849945395,-1.54323678801712));
#8284=CARTESIAN_POINT('Ctrl Pts',(18.7858124404394,-44.7143318634069,-1.54279092935624));
#8285=CARTESIAN_POINT('Ctrl Pts',(18.7868021784292,-44.7145725376574,-1.54236366527359));
#8286=CARTESIAN_POINT('Ctrl Pts',(18.7878041612743,-44.7148185849535,-1.54193392585844));
#8287=CARTESIAN_POINT('Ctrl Pts',(18.789307135542,-44.7151876558978,-1.54128931673572));
#8288=CARTESIAN_POINT('Ctrl Pts',(18.7908372641589,-44.7155695477042,-1.54063843407745));
#8289=CARTESIAN_POINT('Ctrl Pts',(18.7925588171132,-44.7160071547615,-1.53991486409862));
#8290=CARTESIAN_POINT('Ctrl Pts',(18.7934195935903,-44.7162259582902,-1.53955307910921));
#8291=CARTESIAN_POINT('Ctrl Pts',(18.7943283140833,-44.7164585734448,-1.53917329091374));
#8292=CARTESIAN_POINT('Ctrl Pts',(18.7953057447759,-44.7167106512364,-1.53876797724112));
#8293=CARTESIAN_POINT('Ctrl Pts',(18.7962831753214,-44.71696272899,-1.53836266362956));
#8294=CARTESIAN_POINT('Ctrl Pts',(18.7973293149979,-44.7172342636307,-1.53793181150032));
#8295=CARTESIAN_POINT('Ctrl Pts',(18.7984650862778,-44.7175312467786,-1.53746858862735));
#8296=CARTESIAN_POINT('Ctrl Pts',(3.62216201968442,-19.8058202438613,-1.94799199564959));
#8297=CARTESIAN_POINT('Ctrl Pts',(3.34425572651223,-20.2137053466864,-1.54490813204841));
#8298=CARTESIAN_POINT('Ctrl Pts',(3.25594179788809,-20.5121292468035,-0.988830267143717));
#8299=CARTESIAN_POINT('Ctrl Pts',(3.16762786926396,-20.8105531469205,-0.432752402239027));
#8300=CARTESIAN_POINT('Ctrl Pts',(3.3076189187292,-20.9771651064803,0.166181422977342));
#8301=CARTESIAN_POINT('Ctrl Pts',(3.44760996819445,-21.1437770660401,0.765115248193711));
#8302=CARTESIAN_POINT('Ctrl Pts',(3.80940000840298,-21.1823333185883,1.28827884419634));
#8303=CARTESIAN_POINT('Ctrl Pts',(4.17119004861151,-21.2208895711365,1.81144244019896));
#8304=CARTESIAN_POINT('Ctrl Pts',(4.70434308191443,-21.1605093534924,2.15521684061908));
#8305=CARTESIAN_POINT('Ctrl Pts',(5.23749611521735,-21.1001291358485,2.49899124103919));
#8306=CARTESIAN_POINT('Ctrl Pts',(5.8576356015542,-20.9895272661294,2.59528770975726));
#8307=CARTESIAN_POINT('Ctrl Pts',(6.47777508789106,-20.8789253964104,2.69158417847533));
#8308=CARTESIAN_POINT('Ctrl Pts',(7.08329575335921,-20.7767637068552,2.52133001886304));
#8309=CARTESIAN_POINT('Ctrl Pts',(7.68881641882736,-20.6746020173,2.35107585925076));
#8310=CARTESIAN_POINT('Ctrl Pts',(8.18100842628526,-20.6378706589539,1.94799199564959));
#8311=CARTESIAN_POINT('Ctrl Pts',(8.67320043374317,-20.6011393006078,1.54490813204841));
#8312=CARTESIAN_POINT('Ctrl Pts',(8.97580007665302,-20.6738691449698,0.988830267143717));
#8313=CARTESIAN_POINT('Ctrl Pts',(9.27839971956287,-20.7465989893318,0.432752402239027));
#8314=CARTESIAN_POINT('Ctrl Pts',(9.35269438438334,-20.9511407742511,-0.166181422977342));
#8315=CARTESIAN_POINT('Ctrl Pts',(9.4269890492038,-21.1556825591703,-0.765115248193711));
#8316=CARTESIAN_POINT('Ctrl Pts',(9.27948472328098,-21.4882800511012,-1.28827884419634));
#8317=CARTESIAN_POINT('Ctrl Pts',(9.13198039735816,-21.8208775430321,-1.81144244019896));
#8318=CARTESIAN_POINT('Ctrl Pts',(8.81311307834095,-22.2524115051551,-2.15521684061908));
#8319=CARTESIAN_POINT('Ctrl Pts',(8.49424575932375,-22.6839454672782,-2.49899124103919));
#8320=CARTESIAN_POINT('Ctrl Pts',(8.0883919872726,-23.1657010814762,-2.59528770975726));
#8321=CARTESIAN_POINT('Ctrl Pts',(7.68253821522146,-23.6474566956743,-2.69158417847533));
#8322=CARTESIAN_POINT('Ctrl Pts',(7.29130326403902,-24.1207721297085,-2.52133001886305));
#8323=CARTESIAN_POINT('Ctrl Pts',(6.90006831285659,-24.5940875637428,-2.35107585925076));
#8324=CARTESIAN_POINT('Ctrl Pts',(6.62216201968439,-25.0019726665679,-1.94799199564959));
#8325=CARTESIAN_POINT('Ctrl Pts',(6.34425572651219,-25.4098577693931,-1.54490813204841));
#8326=CARTESIAN_POINT('Ctrl Pts',(6.25594179788806,-25.7082816695101,-0.988830267143717));
#8327=CARTESIAN_POINT('Ctrl Pts',(6.16762786926392,-26.0067055696272,-0.432752402239027));
#8328=CARTESIAN_POINT('Ctrl Pts',(6.30761891872917,-26.1733175291869,0.166181422977342));
#8329=CARTESIAN_POINT('Ctrl Pts',(6.44760996819441,-26.3399294887468,0.765115248193711));
#8330=CARTESIAN_POINT('Ctrl Pts',(6.80940000840295,-26.3784857412949,1.28827884419634));
#8331=CARTESIAN_POINT('Ctrl Pts',(7.17119004861148,-26.4170419938431,1.81144244019896));
#8332=CARTESIAN_POINT('Ctrl Pts',(7.7043430819144,-26.3566617761991,2.15521684061908));
#8333=CARTESIAN_POINT('Ctrl Pts',(8.23749611521731,-26.2962815585551,2.49899124103919));
#8334=CARTESIAN_POINT('Ctrl Pts',(8.85763560155417,-26.1856796888361,2.59528770975726));
#8335=CARTESIAN_POINT('Ctrl Pts',(9.47777508789103,-26.0750778191171,2.69158417847533));
#8336=CARTESIAN_POINT('Ctrl Pts',(10.0832957533592,-25.9729161295619,2.52133001886304));
#8337=CARTESIAN_POINT('Ctrl Pts',(10.6888164188273,-25.8707544400067,2.35107585925076));
#8338=CARTESIAN_POINT('Ctrl Pts',(11.1810084262852,-25.8340230816606,1.94799199564959));
#8339=CARTESIAN_POINT('Ctrl Pts',(11.6732004337431,-25.7972917233145,1.54490813204841));
#8340=CARTESIAN_POINT('Ctrl Pts',(11.975800076653,-25.8700215676765,0.988830267143717));
#8341=CARTESIAN_POINT('Ctrl Pts',(12.2783997195628,-25.9427514120385,0.432752402239027));
#8342=CARTESIAN_POINT('Ctrl Pts',(12.3526943843833,-26.1472931969577,-0.166181422977342));
#8343=CARTESIAN_POINT('Ctrl Pts',(12.4269890492038,-26.351834981877,-0.765115248193711));
#8344=CARTESIAN_POINT('Ctrl Pts',(12.279484723281,-26.6844324738078,-1.28827884419634));
#8345=CARTESIAN_POINT('Ctrl Pts',(12.1319803973581,-27.0170299657387,-1.81144244019896));
#8346=CARTESIAN_POINT('Ctrl Pts',(11.8131130783409,-27.4485639278618,-2.15521684061908));
#8347=CARTESIAN_POINT('Ctrl Pts',(11.4942457593237,-27.8800978899848,-2.49899124103919));
#8348=CARTESIAN_POINT('Ctrl Pts',(11.0883919872726,-28.3618535041829,-2.59528770975726));
#8349=CARTESIAN_POINT('Ctrl Pts',(10.6825382152214,-28.8436091183809,-2.69158417847533));
#8350=CARTESIAN_POINT('Ctrl Pts',(10.291303264039,-29.3169245524152,-2.52133001886305));
#8351=CARTESIAN_POINT('Ctrl Pts',(9.90006831285655,-29.7902399864494,-2.35107585925076));
#8352=CARTESIAN_POINT('Ctrl Pts',(9.62216201968436,-30.1981250892746,-1.94799199564959));
#8353=CARTESIAN_POINT('Ctrl Pts',(9.34425572651217,-30.6060101920997,-1.54490813204841));
#8354=CARTESIAN_POINT('Ctrl Pts',(9.25594179788803,-30.9044340922168,-0.988830267143717));
#8355=CARTESIAN_POINT('Ctrl Pts',(9.16762786926389,-31.2028579923338,-0.432752402239027));
#8356=CARTESIAN_POINT('Ctrl Pts',(9.30761891872914,-31.3694699518936,0.166181422977342));
#8357=CARTESIAN_POINT('Ctrl Pts',(9.44760996819438,-31.5360819114534,0.765115248193711));
#8358=CARTESIAN_POINT('Ctrl Pts',(9.80940000840292,-31.5746381640016,1.28827884419634));
#8359=CARTESIAN_POINT('Ctrl Pts',(10.1711900486115,-31.6131944165497,1.81144244019896));
#8360=CARTESIAN_POINT('Ctrl Pts',(10.7043430819144,-31.5528141989058,2.15521684061908));
#8361=CARTESIAN_POINT('Ctrl Pts',(11.2374961152173,-31.4924339812617,2.49899124103919));
#8362=CARTESIAN_POINT('Ctrl Pts',(11.8576356015541,-31.3818321115427,2.59528770975726));
#8363=CARTESIAN_POINT('Ctrl Pts',(12.477775087891,-31.2712302418237,2.69158417847533));
#8364=CARTESIAN_POINT('Ctrl Pts',(13.0832957533591,-31.1690685522685,2.52133001886304));
#8365=CARTESIAN_POINT('Ctrl Pts',(13.6888164188273,-31.0669068627133,2.35107585925076));
#8366=CARTESIAN_POINT('Ctrl Pts',(14.1810084262852,-31.0301755043672,1.94799199564959));
#8367=CARTESIAN_POINT('Ctrl Pts',(14.6732004337431,-30.9934441460211,1.54490813204841));
#8368=CARTESIAN_POINT('Ctrl Pts',(14.975800076653,-31.0661739903831,0.988830267143717));
#8369=CARTESIAN_POINT('Ctrl Pts',(15.2783997195628,-31.1389038347451,0.432752402239027));
#8370=CARTESIAN_POINT('Ctrl Pts',(15.3526943843833,-31.3434456196644,-0.166181422977342));
#8371=CARTESIAN_POINT('Ctrl Pts',(15.4269890492037,-31.5479874045836,-0.765115248193711));
#8372=CARTESIAN_POINT('Ctrl Pts',(15.2794847232809,-31.8805848965145,-1.28827884419634));
#8373=CARTESIAN_POINT('Ctrl Pts',(15.1319803973581,-32.2131823884454,-1.81144244019896));
#8374=CARTESIAN_POINT('Ctrl Pts',(14.8131130783409,-32.6447163505684,-2.15521684061908));
#8375=CARTESIAN_POINT('Ctrl Pts',(14.4942457593237,-33.0762503126915,-2.49899124103919));
#8376=CARTESIAN_POINT('Ctrl Pts',(14.0883919872725,-33.5580059268895,-2.59528770975726));
#8377=CARTESIAN_POINT('Ctrl Pts',(13.6825382152214,-34.0397615410876,-2.69158417847533));
#8378=CARTESIAN_POINT('Ctrl Pts',(13.291303264039,-34.5130769751218,-2.52133001886305));
#8379=CARTESIAN_POINT('Ctrl Pts',(12.9000683128565,-34.9863924091561,-2.35107585925076));
#8380=CARTESIAN_POINT('Ctrl Pts',(12.6221620196843,-35.3942775119812,-1.94799199564959));
#8381=CARTESIAN_POINT('Ctrl Pts',(12.3442557265121,-35.8021626148064,-1.54490813204841));
#8382=CARTESIAN_POINT('Ctrl Pts',(12.255941797888,-36.1005865149234,-0.988830267143717));
#8383=CARTESIAN_POINT('Ctrl Pts',(12.1676278692639,-36.3990104150405,-0.432752402239027));
#8384=CARTESIAN_POINT('Ctrl Pts',(12.3076189187291,-36.5656223746002,0.166181422977342));
#8385=CARTESIAN_POINT('Ctrl Pts',(12.4476099681944,-36.73223433416,0.765115248193711));
#8386=CARTESIAN_POINT('Ctrl Pts',(12.8094000084029,-36.7707905867082,1.28827884419634));
#8387=CARTESIAN_POINT('Ctrl Pts',(13.1711900486114,-36.8093468392564,1.81144244019896));
#8388=CARTESIAN_POINT('Ctrl Pts',(13.7043430819143,-36.7489666216124,2.15521684061908));
#8389=CARTESIAN_POINT('Ctrl Pts',(14.2374961152173,-36.6885864039684,2.49899124103919));
#8390=CARTESIAN_POINT('Ctrl Pts',(14.8576356015541,-36.5779845342494,2.59528770975726));
#8391=CARTESIAN_POINT('Ctrl Pts',(15.477775087891,-36.4673826645304,2.69158417847533));
#8392=CARTESIAN_POINT('Ctrl Pts',(16.0832957533591,-36.3652209749752,2.52133001886304));
#8393=CARTESIAN_POINT('Ctrl Pts',(16.6888164188273,-36.26305928542,2.35107585925076));
#8394=CARTESIAN_POINT('Ctrl Pts',(17.1810084262852,-36.2263279270739,1.94799199564959));
#8395=CARTESIAN_POINT('Ctrl Pts',(17.6732004337431,-36.1895965687278,1.54490813204841));
#8396=CARTESIAN_POINT('Ctrl Pts',(17.9758000766529,-36.2623264130898,0.988830267143717));
#8397=CARTESIAN_POINT('Ctrl Pts',(18.2783997195628,-36.3350562574518,0.432752402239027));
#8398=CARTESIAN_POINT('Ctrl Pts',(18.3526943843832,-36.539598042371,-0.166181422977342));
#8399=CARTESIAN_POINT('Ctrl Pts',(18.4269890492037,-36.7441398272903,-0.765115248193711));
#8400=CARTESIAN_POINT('Ctrl Pts',(18.2794847232809,-37.0767373192211,-1.28827884419634));
#8401=CARTESIAN_POINT('Ctrl Pts',(18.1319803973581,-37.409334811152,-1.81144244019896));
#8402=CARTESIAN_POINT('Ctrl Pts',(17.8131130783409,-37.8408687732751,-2.15521684061908));
#8403=CARTESIAN_POINT('Ctrl Pts',(17.4942457593237,-38.2724027353981,-2.49899124103919));
#8404=CARTESIAN_POINT('Ctrl Pts',(17.0883919872725,-38.7541583495962,-2.59528770975726));
#8405=CARTESIAN_POINT('Ctrl Pts',(16.6825382152214,-39.2359139637942,-2.69158417847533));
#8406=CARTESIAN_POINT('Ctrl Pts',(16.2913032640389,-39.7092293978285,-2.52133001886305));
#8407=CARTESIAN_POINT('Ctrl Pts',(15.9000683128565,-40.1825448318627,-2.35107585925076));
#8408=CARTESIAN_POINT('Ctrl Pts',(15.6221620196843,-40.5904299346879,-1.94799199564959));
#8409=CARTESIAN_POINT('Ctrl Pts',(15.3442557265121,-40.998315037513,-1.54490813204841));
#8410=CARTESIAN_POINT('Ctrl Pts',(15.255941797888,-41.2967389376301,-0.988830267143717));
#8411=CARTESIAN_POINT('Ctrl Pts',(15.1676278692638,-41.5951628377471,-0.432752402239027));
#8412=CARTESIAN_POINT('Ctrl Pts',(15.3076189187291,-41.7617747973069,0.166181422977342));
#8413=CARTESIAN_POINT('Ctrl Pts',(15.4476099681943,-41.9283867568667,0.765115248193711));
#8414=CARTESIAN_POINT('Ctrl Pts',(15.8094000084029,-41.9669430094149,1.28827884419634));
#8415=CARTESIAN_POINT('Ctrl Pts',(16.1711900486114,-42.0054992619631,1.81144244019896));
#8416=CARTESIAN_POINT('Ctrl Pts',(16.7043430819143,-41.945119044319,2.15521684061908));
#8417=CARTESIAN_POINT('Ctrl Pts',(17.2374961152172,-41.884738826675,2.49899124103919));
#8418=CARTESIAN_POINT('Ctrl Pts',(17.8576356015541,-41.774136956956,2.59528770975726));
#8419=CARTESIAN_POINT('Ctrl Pts',(18.4777750878909,-41.6635350872371,2.69158417847533));
#8420=CARTESIAN_POINT('Ctrl Pts',(19.0832957533591,-41.5613733976818,2.52133001886304));
#8421=CARTESIAN_POINT('Ctrl Pts',(19.6888164188272,-41.4592117081266,2.35107585925076));
#8422=CARTESIAN_POINT('Ctrl Pts',(20.1810084262851,-41.4224803497805,1.94799199564959));
#8423=CARTESIAN_POINT('Ctrl Pts',(20.673200433743,-41.3857489914344,1.54490813204841));
#8424=CARTESIAN_POINT('Ctrl Pts',(20.9758000766529,-41.4584788357964,0.988830267143717));
#8425=CARTESIAN_POINT('Ctrl Pts',(21.2783997195627,-41.5312086801584,0.432752402239027));
#8426=CARTESIAN_POINT('Ctrl Pts',(21.3526943843832,-41.7357504650777,-0.166181422977342));
#8427=CARTESIAN_POINT('Ctrl Pts',(21.4269890492037,-41.940292249997,-0.765115248193711));
#8428=CARTESIAN_POINT('Ctrl Pts',(21.2794847232809,-42.2728897419278,-1.28827884419634));
#8429=CARTESIAN_POINT('Ctrl Pts',(21.131980397358,-42.6054872338587,-1.81144244019896));
#8430=CARTESIAN_POINT('Ctrl Pts',(20.8131130783408,-43.0370211959817,-2.15521684061908));
#8431=CARTESIAN_POINT('Ctrl Pts',(20.4942457593236,-43.4685551581048,-2.49899124103919));
#8432=CARTESIAN_POINT('Ctrl Pts',(20.0883919872725,-43.9503107723028,-2.59528770975726));
#8433=CARTESIAN_POINT('Ctrl Pts',(19.6825382152213,-44.4320663865008,-2.69158417847533));
#8434=CARTESIAN_POINT('Ctrl Pts',(19.2913032640389,-44.9053818205351,-2.52133001886305));
#8435=CARTESIAN_POINT('Ctrl Pts',(18.9000683128565,-45.3786972545694,-2.35107585925076));
#8436=CARTESIAN_POINT('Ctrl Pts',(18.6221620196843,-45.7865823573945,-1.94799199564959));
#8437=CARTESIAN_POINT('Ctrl Pts',(4.55184415422078,-20.0688325405066,-1.69008569379309));
#8438=CARTESIAN_POINT('Ctrl Pts',(4.32491681918215,-20.4472849281303,-1.4407517010054));
#8439=CARTESIAN_POINT('Ctrl Pts',(4.22476116346577,-20.7525456525717,-1.04873843619563));
#8440=CARTESIAN_POINT('Ctrl Pts',(4.12460550774938,-21.0578063770131,-0.656725171385866));
#8441=CARTESIAN_POINT('Ctrl Pts',(4.19227954417643,-21.2661705835175,-0.199675669376779));
#8442=CARTESIAN_POINT('Ctrl Pts',(4.25995358060348,-21.4745347900219,0.257373832632308));
#8443=CARTESIAN_POINT('Ctrl Pts',(4.50327459317005,-21.5814891675698,0.688935312623524));
#8444=CARTESIAN_POINT('Ctrl Pts',(4.74659560573663,-21.6884435451177,1.12049679261474));
#8445=CARTESIAN_POINT('Ctrl Pts',(5.13859184064558,-21.7095602430244,1.44109420672161));
#8446=CARTESIAN_POINT('Ctrl Pts',(5.53058807555453,-21.7306769409311,1.76169162082848));
#8447=CARTESIAN_POINT('Ctrl Pts',(6.01484082784187,-21.6985293136949,1.90782671931788));
#8448=CARTESIAN_POINT('Ctrl Pts',(6.49909358012921,-21.6663816864587,2.05396181780729));
#8449=CARTESIAN_POINT('Ctrl Pts',(7.00091161011221,-21.6240927414165,1.99669075219403));
#8450=CARTESIAN_POINT('Ctrl Pts',(7.50272964009522,-21.5818037963743,1.93941968658077));
#8451=CARTESIAN_POINT('Ctrl Pts',(7.94394268941957,-21.5745051532296,1.69008569379309));
#8452=CARTESIAN_POINT('Ctrl Pts',(8.38515573874391,-21.5672065100849,1.4407517010054));
#8453=CARTESIAN_POINT('Ctrl Pts',(8.699597108746,-21.6330995301225,1.04873843619563));
#8454=CARTESIAN_POINT('Ctrl Pts',(9.0140384787481,-21.6989925501602,0.656725171385866));
#8455=CARTESIAN_POINT('Ctrl Pts',(9.16065015660677,-21.8617820881348,0.199675669376779));
#8456=CARTESIAN_POINT('Ctrl Pts',(9.30726183446543,-22.0245716261095,-0.257373832632308));
#8457=CARTESIAN_POINT('Ctrl Pts',(9.27822653618457,-22.2887709930406,-0.688935312623524));
#8458=CARTESIAN_POINT('Ctrl Pts',(9.24919123790371,-22.5529703599718,-1.12049679261474));
#8459=CARTESIAN_POINT('Ctrl Pts',(9.07148071728047,-22.9030074065441,-1.44109420672161));
#8460=CARTESIAN_POINT('Ctrl Pts',(8.89377019665723,-23.2530444531165,-1.76169162082848));
#8461=CARTESIAN_POINT('Ctrl Pts',(8.6238031586556,-23.6563458248317,-1.90782671931788));
#8462=CARTESIAN_POINT('Ctrl Pts',(8.35383612065398,-24.059647196547,-2.05396181780729));
#8463=CARTESIAN_POINT('Ctrl Pts',(8.06630380495668,-24.4730898860682,-1.99669075219403));
#8464=CARTESIAN_POINT('Ctrl Pts',(7.77877148925938,-24.8865325755895,-1.93941968658077));
#8465=CARTESIAN_POINT('Ctrl Pts',(7.55184415422075,-25.2649849632132,-1.69008569379309));
#8466=CARTESIAN_POINT('Ctrl Pts',(7.32491681918212,-25.6434373508369,-1.4407517010054));
#8467=CARTESIAN_POINT('Ctrl Pts',(7.22476116346574,-25.9486980752784,-1.04873843619563));
#8468=CARTESIAN_POINT('Ctrl Pts',(7.12460550774935,-26.2539587997198,-0.656725171385866));
#8469=CARTESIAN_POINT('Ctrl Pts',(7.1922795441764,-26.4623230062242,-0.199675669376779));
#8470=CARTESIAN_POINT('Ctrl Pts',(7.25995358060345,-26.6706872127285,0.257373832632308));
#8471=CARTESIAN_POINT('Ctrl Pts',(7.50327459317002,-26.7776415902764,0.688935312623524));
#8472=CARTESIAN_POINT('Ctrl Pts',(7.7465956057366,-26.8845959678243,1.12049679261474));
#8473=CARTESIAN_POINT('Ctrl Pts',(8.13859184064555,-26.905712665731,1.44109420672161));
#8474=CARTESIAN_POINT('Ctrl Pts',(8.5305880755545,-26.9268293636377,1.76169162082848));
#8475=CARTESIAN_POINT('Ctrl Pts',(9.01484082784184,-26.8946817364015,1.90782671931788));
#8476=CARTESIAN_POINT('Ctrl Pts',(9.49909358012917,-26.8625341091653,2.05396181780729));
#8477=CARTESIAN_POINT('Ctrl Pts',(10.0009116101122,-26.8202451641231,1.99669075219403));
#8478=CARTESIAN_POINT('Ctrl Pts',(10.5027296400952,-26.7779562190809,1.93941968658077));
#8479=CARTESIAN_POINT('Ctrl Pts',(10.9439426894195,-26.7706575759362,1.69008569379309));
#8480=CARTESIAN_POINT('Ctrl Pts',(11.3851557387439,-26.7633589327915,1.4407517010054));
#8481=CARTESIAN_POINT('Ctrl Pts',(11.699597108746,-26.8292519528292,1.04873843619563));
#8482=CARTESIAN_POINT('Ctrl Pts',(12.0140384787481,-26.8951449728668,0.656725171385866));
#8483=CARTESIAN_POINT('Ctrl Pts',(12.1606501566067,-27.0579345108415,0.199675669376779));
#8484=CARTESIAN_POINT('Ctrl Pts',(12.3072618344654,-27.2207240488161,-0.257373832632308));
#8485=CARTESIAN_POINT('Ctrl Pts',(12.2782265361845,-27.4849234157473,-0.688935312623524));
#8486=CARTESIAN_POINT('Ctrl Pts',(12.2491912379037,-27.7491227826784,-1.12049679261474));
#8487=CARTESIAN_POINT('Ctrl Pts',(12.0714807172804,-28.0991598292508,-1.44109420672161));
#8488=CARTESIAN_POINT('Ctrl Pts',(11.8937701966572,-28.4491968758231,-1.76169162082848));
#8489=CARTESIAN_POINT('Ctrl Pts',(11.6238031586556,-28.8524982475384,-1.90782671931788));
#8490=CARTESIAN_POINT('Ctrl Pts',(11.3538361206539,-29.2557996192536,-2.05396181780729));
#8491=CARTESIAN_POINT('Ctrl Pts',(11.0663038049567,-29.6692423087749,-1.99669075219403));
#8492=CARTESIAN_POINT('Ctrl Pts',(10.7787714892594,-30.0826849982961,-1.93941968658077));
#8493=CARTESIAN_POINT('Ctrl Pts',(10.5518441542207,-30.4611373859199,-1.69008569379309));
#8494=CARTESIAN_POINT('Ctrl Pts',(10.3249168191821,-30.8395897735436,-1.4407517010054));
#8495=CARTESIAN_POINT('Ctrl Pts',(10.2247611634657,-31.144850497985,-1.04873843619563));
#8496=CARTESIAN_POINT('Ctrl Pts',(10.1246055077493,-31.4501112224264,-0.656725171385866));
#8497=CARTESIAN_POINT('Ctrl Pts',(10.1922795441764,-31.6584754289308,-0.199675669376779));
#8498=CARTESIAN_POINT('Ctrl Pts',(10.2599535806034,-31.8668396354352,0.257373832632308));
#8499=CARTESIAN_POINT('Ctrl Pts',(10.50327459317,-31.9737940129831,0.688935312623524));
#8500=CARTESIAN_POINT('Ctrl Pts',(10.7465956057366,-32.080748390531,1.12049679261474));
#8501=CARTESIAN_POINT('Ctrl Pts',(11.1385918406455,-32.1018650884377,1.44109420672161));
#8502=CARTESIAN_POINT('Ctrl Pts',(11.5305880755545,-32.1229817863444,1.76169162082848));
#8503=CARTESIAN_POINT('Ctrl Pts',(12.0148408278418,-32.0908341591082,1.90782671931788));
#8504=CARTESIAN_POINT('Ctrl Pts',(12.4990935801291,-32.0586865318719,2.05396181780729));
#8505=CARTESIAN_POINT('Ctrl Pts',(13.0009116101121,-32.0163975868298,1.99669075219403));
#8506=CARTESIAN_POINT('Ctrl Pts',(13.5027296400952,-31.9741086417876,1.93941968658077));
#8507=CARTESIAN_POINT('Ctrl Pts',(13.9439426894195,-31.9668099986429,1.69008569379309));
#8508=CARTESIAN_POINT('Ctrl Pts',(14.3851557387438,-31.9595113554982,1.4407517010054));
#8509=CARTESIAN_POINT('Ctrl Pts',(14.6995971087459,-32.0254043755358,1.04873843619563));
#8510=CARTESIAN_POINT('Ctrl Pts',(15.014038478748,-32.0912973955735,0.656725171385866));
#8511=CARTESIAN_POINT('Ctrl Pts',(15.1606501566067,-32.2540869335481,0.199675669376779));
#8512=CARTESIAN_POINT('Ctrl Pts',(15.3072618344654,-32.4168764715228,-0.257373832632308));
#8513=CARTESIAN_POINT('Ctrl Pts',(15.2782265361845,-32.6810758384539,-0.688935312623524));
#8514=CARTESIAN_POINT('Ctrl Pts',(15.2491912379036,-32.9452752053851,-1.12049679261474));
#8515=CARTESIAN_POINT('Ctrl Pts',(15.0714807172804,-33.2953122519574,-1.44109420672161));
#8516=CARTESIAN_POINT('Ctrl Pts',(14.8937701966572,-33.6453492985298,-1.76169162082848));
#8517=CARTESIAN_POINT('Ctrl Pts',(14.6238031586555,-34.048650670245,-1.90782671931788));
#8518=CARTESIAN_POINT('Ctrl Pts',(14.3538361206539,-34.4519520419603,-2.05396181780729));
#8519=CARTESIAN_POINT('Ctrl Pts',(14.0663038049566,-34.8653947314815,-1.99669075219403));
#8520=CARTESIAN_POINT('Ctrl Pts',(13.7787714892593,-35.2788374210028,-1.93941968658077));
#8521=CARTESIAN_POINT('Ctrl Pts',(13.5518441542207,-35.6572898086265,-1.69008569379309));
#8522=CARTESIAN_POINT('Ctrl Pts',(13.3249168191821,-36.0357421962502,-1.4407517010054));
#8523=CARTESIAN_POINT('Ctrl Pts',(13.2247611634657,-36.3410029206916,-1.04873843619563));
#8524=CARTESIAN_POINT('Ctrl Pts',(13.1246055077493,-36.6462636451331,-0.656725171385866));
#8525=CARTESIAN_POINT('Ctrl Pts',(13.1922795441763,-36.8546278516375,-0.199675669376779));
#8526=CARTESIAN_POINT('Ctrl Pts',(13.2599535806034,-37.0629920581418,0.257373832632308));
#8527=CARTESIAN_POINT('Ctrl Pts',(13.50327459317,-37.1699464356897,0.688935312623524));
#8528=CARTESIAN_POINT('Ctrl Pts',(13.7465956057365,-37.2769008132376,1.12049679261474));
#8529=CARTESIAN_POINT('Ctrl Pts',(14.1385918406455,-37.2980175111443,1.44109420672161));
#8530=CARTESIAN_POINT('Ctrl Pts',(14.5305880755544,-37.319134209051,1.76169162082848));
#8531=CARTESIAN_POINT('Ctrl Pts',(15.0148408278418,-37.2869865818148,1.90782671931788));
#8532=CARTESIAN_POINT('Ctrl Pts',(15.4990935801291,-37.2548389545786,2.05396181780729));
#8533=CARTESIAN_POINT('Ctrl Pts',(16.0009116101121,-37.2125500095364,1.99669075219403));
#8534=CARTESIAN_POINT('Ctrl Pts',(16.5027296400951,-37.1702610644942,1.93941968658077));
#8535=CARTESIAN_POINT('Ctrl Pts',(16.9439426894195,-37.1629624213495,1.69008569379309));
#8536=CARTESIAN_POINT('Ctrl Pts',(17.3851557387438,-37.1556637782049,1.4407517010054));
#8537=CARTESIAN_POINT('Ctrl Pts',(17.6995971087459,-37.2215567982425,1.04873843619563));
#8538=CARTESIAN_POINT('Ctrl Pts',(18.014038478748,-37.2874498182801,0.656725171385866));
#8539=CARTESIAN_POINT('Ctrl Pts',(18.1606501566067,-37.4502393562548,0.199675669376779));
#8540=CARTESIAN_POINT('Ctrl Pts',(18.3072618344653,-37.6130288942294,-0.257373832632308));
#8541=CARTESIAN_POINT('Ctrl Pts',(18.2782265361845,-37.8772282611606,-0.688935312623524));
#8542=CARTESIAN_POINT('Ctrl Pts',(18.2491912379036,-38.1414276280917,-1.12049679261474));
#8543=CARTESIAN_POINT('Ctrl Pts',(18.0714807172804,-38.4914646746641,-1.44109420672161));
#8544=CARTESIAN_POINT('Ctrl Pts',(17.8937701966571,-38.8415017212364,-1.76169162082848));
#8545=CARTESIAN_POINT('Ctrl Pts',(17.6238031586555,-39.2448030929517,-1.90782671931788));
#8546=CARTESIAN_POINT('Ctrl Pts',(17.3538361206539,-39.6481044646669,-2.05396181780729));
#8547=CARTESIAN_POINT('Ctrl Pts',(17.0663038049566,-40.0615471541882,-1.99669075219403));
#8548=CARTESIAN_POINT('Ctrl Pts',(16.7787714892593,-40.4749898437094,-1.93941968658077));
#8549=CARTESIAN_POINT('Ctrl Pts',(16.5518441542207,-40.8534422313332,-1.69008569379309));
#8550=CARTESIAN_POINT('Ctrl Pts',(16.324916819182,-41.2318946189569,-1.4407517010054));
#8551=CARTESIAN_POINT('Ctrl Pts',(16.2247611634656,-41.5371553433983,-1.04873843619563));
#8552=CARTESIAN_POINT('Ctrl Pts',(16.1246055077493,-41.8424160678397,-0.656725171385866));
#8553=CARTESIAN_POINT('Ctrl Pts',(16.1922795441763,-42.0507802743441,-0.199675669376779));
#8554=CARTESIAN_POINT('Ctrl Pts',(16.2599535806034,-42.2591444808485,0.257373832632308));
#8555=CARTESIAN_POINT('Ctrl Pts',(16.5032745931699,-42.3660988583964,0.688935312623524));
#8556=CARTESIAN_POINT('Ctrl Pts',(16.7465956057365,-42.4730532359443,1.12049679261474));
#8557=CARTESIAN_POINT('Ctrl Pts',(17.1385918406455,-42.494169933851,1.44109420672161));
#8558=CARTESIAN_POINT('Ctrl Pts',(17.5305880755544,-42.5152866317577,1.76169162082848));
#8559=CARTESIAN_POINT('Ctrl Pts',(18.0148408278417,-42.4831390045215,1.90782671931788));
#8560=CARTESIAN_POINT('Ctrl Pts',(18.4990935801291,-42.4509913772853,2.05396181780729));
#8561=CARTESIAN_POINT('Ctrl Pts',(19.0009116101121,-42.4087024322431,1.99669075219403));
#8562=CARTESIAN_POINT('Ctrl Pts',(19.5027296400951,-42.3664134872009,1.93941968658077));
#8563=CARTESIAN_POINT('Ctrl Pts',(19.9439426894194,-42.3591148440562,1.69008569379309));
#8564=CARTESIAN_POINT('Ctrl Pts',(20.3851557387438,-42.3518162009115,1.4407517010054));
#8565=CARTESIAN_POINT('Ctrl Pts',(20.6995971087459,-42.4177092209491,1.04873843619563));
#8566=CARTESIAN_POINT('Ctrl Pts',(21.014038478748,-42.4836022409868,0.656725171385866));
#8567=CARTESIAN_POINT('Ctrl Pts',(21.1606501566066,-42.6463917789614,0.199675669376779));
#8568=CARTESIAN_POINT('Ctrl Pts',(21.3072618344653,-42.8091813169361,-0.257373832632308));
#8569=CARTESIAN_POINT('Ctrl Pts',(21.2782265361844,-43.0733806838672,-0.688935312623524));
#8570=CARTESIAN_POINT('Ctrl Pts',(21.2491912379036,-43.3375800507984,-1.12049679261474));
#8571=CARTESIAN_POINT('Ctrl Pts',(21.0714807172803,-43.6876170973707,-1.44109420672161));
#8572=CARTESIAN_POINT('Ctrl Pts',(20.8937701966571,-44.0376541439431,-1.76169162082848));
#8573=CARTESIAN_POINT('Ctrl Pts',(20.6238031586555,-44.4409555156583,-1.90782671931788));
#8574=CARTESIAN_POINT('Ctrl Pts',(20.3538361206538,-44.8442568873736,-2.05396181780729));
#8575=CARTESIAN_POINT('Ctrl Pts',(20.0663038049566,-45.2576995768948,-1.99669075219403));
#8576=CARTESIAN_POINT('Ctrl Pts',(19.7787714892593,-45.6711422664161,-1.93941968658077));
#8577=CARTESIAN_POINT('Ctrl Pts',(19.5518441542206,-46.0495946540398,-1.69008569379309));
#8578=CARTESIAN_POINT('Ctrl Pts',(4.55184415422078,-19.3686903861425,-0.976082217833403));
#8579=CARTESIAN_POINT('Ctrl Pts',(4.4660500642644,-19.6656594567264,-0.80664966398524));
#8580=CARTESIAN_POINT('Ctrl Pts',(4.46302775611024,-19.9148402168055,-0.557333680706485));
#8581=CARTESIAN_POINT('Ctrl Pts',(4.46000544795609,-20.1640209768846,-0.30801769742773));
#8582=CARTESIAN_POINT('Ctrl Pts',(4.56157448367832,-20.3528158964217,-0.0281983728666175));
#8583=CARTESIAN_POINT('Ctrl Pts',(4.66314351940055,-20.5416108159588,0.251620951694495));
#8584=CARTESIAN_POINT('Ctrl Pts',(4.87040786268996,-20.66938252122,0.506521968549832));
#8585=CARTESIAN_POINT('Ctrl Pts',(5.07767220597936,-20.7971542264811,0.761422985405168));
#8586=CARTESIAN_POINT('Ctrl Pts',(5.37080156859517,-20.8753517397202,0.940919422010711));
#8587=CARTESIAN_POINT('Ctrl Pts',(5.66393093121099,-20.9535492529593,1.12041585861625));
#8588=CARTESIAN_POINT('Ctrl Pts',(6.00608840476948,-21.0034403731477,1.18895624432295));
#8589=CARTESIAN_POINT('Ctrl Pts',(6.34824587832798,-21.0533314933362,1.25749663002964));
#8590=CARTESIAN_POINT('Ctrl Pts',(6.69288393578292,-21.1017904477443,1.2015057008556));
#8591=CARTESIAN_POINT('Ctrl Pts',(7.03752199323787,-21.1502494021524,1.14551477168157));
#8592=CARTESIAN_POINT('Ctrl Pts',(7.33760179747996,-21.2244340760476,0.976082217833403));
#8593=CARTESIAN_POINT('Ctrl Pts',(7.63768160172206,-21.2986187499427,0.80664966398524));
#8594=CARTESIAN_POINT('Ctrl Pts',(7.85498962416192,-21.4205917343427,0.557333680706485));
#8595=CARTESIAN_POINT('Ctrl Pts',(8.07229764660179,-21.5425647187427,0.308017697427731));
#8596=CARTESIAN_POINT('Ctrl Pts',(8.18501432516527,-21.7249235436846,0.0281983728666177));
#8597=CARTESIAN_POINT('Ctrl Pts',(8.29773100372875,-21.9072823686265,-0.251620951694495));
#8598=CARTESIAN_POINT('Ctrl Pts',(8.30475237472506,-22.1506644078444,-0.506521968549832));
#8599=CARTESIAN_POINT('Ctrl Pts',(8.31177374572137,-22.3940464470623,-0.761422985405168));
#8600=CARTESIAN_POINT('Ctrl Pts',(8.23293009739127,-22.6870026783022,-0.940919422010711));
#8601=CARTESIAN_POINT('Ctrl Pts',(8.15408644906117,-22.9799589095422,-1.12041585861625));
#8602=CARTESIAN_POINT('Ctrl Pts',(8.02621468978838,-23.3012215338328,-1.18895624432295));
#8603=CARTESIAN_POINT('Ctrl Pts',(7.8983429305156,-23.6224841581234,-1.25749663002964));
#8604=CARTESIAN_POINT('Ctrl Pts',(7.76799058734637,-23.9451789481943,-1.2015057008556));
#8605=CARTESIAN_POINT('Ctrl Pts',(7.63763824417713,-24.2678737382653,-1.14551477168157));
#8606=CARTESIAN_POINT('Ctrl Pts',(7.55184415422075,-24.5648428088492,-0.976082217833403));
#8607=CARTESIAN_POINT('Ctrl Pts',(7.46605006426437,-24.8618118794331,-0.80664966398524));
#8608=CARTESIAN_POINT('Ctrl Pts',(7.46302775611021,-25.1109926395121,-0.557333680706485));
#8609=CARTESIAN_POINT('Ctrl Pts',(7.46000544795606,-25.3601733995912,-0.30801769742773));
#8610=CARTESIAN_POINT('Ctrl Pts',(7.56157448367829,-25.5489683191283,-0.0281983728666175));
#8611=CARTESIAN_POINT('Ctrl Pts',(7.66314351940052,-25.7377632386655,0.251620951694495));
#8612=CARTESIAN_POINT('Ctrl Pts',(7.87040786268992,-25.8655349439266,0.506521968549832));
#8613=CARTESIAN_POINT('Ctrl Pts',(8.07767220597933,-25.9933066491878,0.761422985405168));
#8614=CARTESIAN_POINT('Ctrl Pts',(8.37080156859514,-26.0715041624269,0.940919422010711));
#8615=CARTESIAN_POINT('Ctrl Pts',(8.66393093121095,-26.1497016756659,1.12041585861625));
#8616=CARTESIAN_POINT('Ctrl Pts',(9.00608840476945,-26.1995927958544,1.18895624432295));
#8617=CARTESIAN_POINT('Ctrl Pts',(9.34824587832795,-26.2494839160429,1.25749663002964));
#8618=CARTESIAN_POINT('Ctrl Pts',(9.69288393578289,-26.297942870451,1.2015057008556));
#8619=CARTESIAN_POINT('Ctrl Pts',(10.0375219932378,-26.346401824859,1.14551477168157));
#8620=CARTESIAN_POINT('Ctrl Pts',(10.3376017974799,-26.4205864987542,0.976082217833403));
#8621=CARTESIAN_POINT('Ctrl Pts',(10.637681601722,-26.4947711726494,0.80664966398524));
#8622=CARTESIAN_POINT('Ctrl Pts',(10.8549896241619,-26.6167441570493,0.557333680706485));
#8623=CARTESIAN_POINT('Ctrl Pts',(11.0722976466018,-26.7387171414493,0.308017697427731));
#8624=CARTESIAN_POINT('Ctrl Pts',(11.1850143251652,-26.9210759663912,0.0281983728666177));
#8625=CARTESIAN_POINT('Ctrl Pts',(11.2977310037287,-27.1034347913331,-0.251620951694495));
#8626=CARTESIAN_POINT('Ctrl Pts',(11.304752374725,-27.346816830551,-0.506521968549832));
#8627=CARTESIAN_POINT('Ctrl Pts',(11.3117737457213,-27.5901988697689,-0.761422985405168));
#8628=CARTESIAN_POINT('Ctrl Pts',(11.2329300973912,-27.8831551010089,-0.940919422010711));
#8629=CARTESIAN_POINT('Ctrl Pts',(11.1540864490611,-28.1761113322489,-1.12041585861625));
#8630=CARTESIAN_POINT('Ctrl Pts',(11.0262146897884,-28.4973739565395,-1.18895624432295));
#8631=CARTESIAN_POINT('Ctrl Pts',(10.8983429305156,-28.8186365808301,-1.25749663002964));
#8632=CARTESIAN_POINT('Ctrl Pts',(10.7679905873463,-29.141331370901,-1.2015057008556));
#8633=CARTESIAN_POINT('Ctrl Pts',(10.6376382441771,-29.4640261609719,-1.14551477168157));
#8634=CARTESIAN_POINT('Ctrl Pts',(10.5518441542207,-29.7609952315558,-0.976082217833403));
#8635=CARTESIAN_POINT('Ctrl Pts',(10.4660500642643,-30.0579643021397,-0.80664966398524));
#8636=CARTESIAN_POINT('Ctrl Pts',(10.4630277561102,-30.3071450622188,-0.557333680706485));
#8637=CARTESIAN_POINT('Ctrl Pts',(10.460005447956,-30.5563258222979,-0.30801769742773));
#8638=CARTESIAN_POINT('Ctrl Pts',(10.5615744836783,-30.745120741835,-0.0281983728666175));
#8639=CARTESIAN_POINT('Ctrl Pts',(10.6631435194005,-30.9339156613721,0.251620951694495));
#8640=CARTESIAN_POINT('Ctrl Pts',(10.8704078626899,-31.0616873666333,0.506521968549832));
#8641=CARTESIAN_POINT('Ctrl Pts',(11.0776722059793,-31.1894590718944,0.761422985405168));
#8642=CARTESIAN_POINT('Ctrl Pts',(11.3708015685951,-31.2676565851335,0.940919422010711));
#8643=CARTESIAN_POINT('Ctrl Pts',(11.6639309312109,-31.3458540983726,1.12041585861625));
#8644=CARTESIAN_POINT('Ctrl Pts',(12.0060884047694,-31.395745218561,1.18895624432295));
#8645=CARTESIAN_POINT('Ctrl Pts',(12.3482458783279,-31.4456363387495,1.25749663002964));
#8646=CARTESIAN_POINT('Ctrl Pts',(12.6928839357829,-31.4940952931576,1.2015057008556));
#8647=CARTESIAN_POINT('Ctrl Pts',(13.0375219932378,-31.5425542475657,1.14551477168157));
#8648=CARTESIAN_POINT('Ctrl Pts',(13.3376017974799,-31.6167389214609,0.976082217833403));
#8649=CARTESIAN_POINT('Ctrl Pts',(13.637681601722,-31.690923595356,0.80664966398524));
#8650=CARTESIAN_POINT('Ctrl Pts',(13.8549896241619,-31.812896579756,0.557333680706485));
#8651=CARTESIAN_POINT('Ctrl Pts',(14.0722976466017,-31.934869564156,0.308017697427731));
#8652=CARTESIAN_POINT('Ctrl Pts',(14.1850143251652,-32.1172283890979,0.0281983728666177));
#8653=CARTESIAN_POINT('Ctrl Pts',(14.2977310037287,-32.2995872140398,-0.251620951694495));
#8654=CARTESIAN_POINT('Ctrl Pts',(14.304752374725,-32.5429692532577,-0.506521968549832));
#8655=CARTESIAN_POINT('Ctrl Pts',(14.3117737457213,-32.7863512924756,-0.761422985405168));
#8656=CARTESIAN_POINT('Ctrl Pts',(14.2329300973912,-33.0793075237155,-0.940919422010711));
#8657=CARTESIAN_POINT('Ctrl Pts',(14.1540864490611,-33.3722637549555,-1.12041585861625));
#8658=CARTESIAN_POINT('Ctrl Pts',(14.0262146897883,-33.6935263792461,-1.18895624432295));
#8659=CARTESIAN_POINT('Ctrl Pts',(13.8983429305155,-34.0147890035367,-1.25749663002964));
#8660=CARTESIAN_POINT('Ctrl Pts',(13.7679905873463,-34.3374837936076,-1.2015057008556));
#8661=CARTESIAN_POINT('Ctrl Pts',(13.6376382441771,-34.6601785836786,-1.14551477168157));
#8662=CARTESIAN_POINT('Ctrl Pts',(13.5518441542207,-34.9571476542625,-0.976082217833403));
#8663=CARTESIAN_POINT('Ctrl Pts',(13.4660500642643,-35.2541167248464,-0.80664966398524));
#8664=CARTESIAN_POINT('Ctrl Pts',(13.4630277561101,-35.5032974849254,-0.557333680706485));
#8665=CARTESIAN_POINT('Ctrl Pts',(13.460005447956,-35.7524782450045,-0.30801769742773));
#8666=CARTESIAN_POINT('Ctrl Pts',(13.5615744836782,-35.9412731645416,-0.0281983728666175));
#8667=CARTESIAN_POINT('Ctrl Pts',(13.6631435194005,-36.1300680840788,0.251620951694495));
#8668=CARTESIAN_POINT('Ctrl Pts',(13.8704078626899,-36.2578397893399,0.506521968549832));
#8669=CARTESIAN_POINT('Ctrl Pts',(14.0776722059793,-36.3856114946011,0.761422985405168));
#8670=CARTESIAN_POINT('Ctrl Pts',(14.3708015685951,-36.4638090078402,0.940919422010711));
#8671=CARTESIAN_POINT('Ctrl Pts',(14.6639309312109,-36.5420065210792,1.12041585861625));
#8672=CARTESIAN_POINT('Ctrl Pts',(15.0060884047694,-36.5918976412677,1.18895624432295));
#8673=CARTESIAN_POINT('Ctrl Pts',(15.3482458783279,-36.6417887614562,1.25749663002964));
#8674=CARTESIAN_POINT('Ctrl Pts',(15.6928839357828,-36.6902477158643,1.2015057008556));
#8675=CARTESIAN_POINT('Ctrl Pts',(16.0375219932378,-36.7387066702723,1.14551477168157));
#8676=CARTESIAN_POINT('Ctrl Pts',(16.3376017974799,-36.8128913441675,0.976082217833403));
#8677=CARTESIAN_POINT('Ctrl Pts',(16.637681601722,-36.8870760180627,0.80664966398524));
#8678=CARTESIAN_POINT('Ctrl Pts',(16.8549896241618,-37.0090490024626,0.557333680706485));
#8679=CARTESIAN_POINT('Ctrl Pts',(17.0722976466017,-37.1310219868626,0.308017697427731));
#8680=CARTESIAN_POINT('Ctrl Pts',(17.1850143251652,-37.3133808118045,0.0281983728666177));
#8681=CARTESIAN_POINT('Ctrl Pts',(17.2977310037287,-37.4957396367464,-0.251620951694495));
#8682=CARTESIAN_POINT('Ctrl Pts',(17.304752374725,-37.7391216759643,-0.506521968549832));
#8683=CARTESIAN_POINT('Ctrl Pts',(17.3117737457213,-37.9825037151822,-0.761422985405168));
#8684=CARTESIAN_POINT('Ctrl Pts',(17.2329300973912,-38.2754599464222,-0.940919422010711));
#8685=CARTESIAN_POINT('Ctrl Pts',(17.1540864490611,-38.5684161776622,-1.12041585861625));
#8686=CARTESIAN_POINT('Ctrl Pts',(17.0262146897883,-38.8896788019527,-1.18895624432295));
#8687=CARTESIAN_POINT('Ctrl Pts',(16.8983429305155,-39.2109414262433,-1.25749663002964));
#8688=CARTESIAN_POINT('Ctrl Pts',(16.7679905873463,-39.5336362163143,-1.2015057008556));
#8689=CARTESIAN_POINT('Ctrl Pts',(16.637638244177,-39.8563310063852,-1.14551477168157));
#8690=CARTESIAN_POINT('Ctrl Pts',(16.5518441542207,-40.1533000769691,-0.976082217833403));
#8691=CARTESIAN_POINT('Ctrl Pts',(16.4660500642643,-40.450269147553,-0.80664966398524));
#8692=CARTESIAN_POINT('Ctrl Pts',(16.4630277561101,-40.6994499076321,-0.557333680706485));
#8693=CARTESIAN_POINT('Ctrl Pts',(16.460005447956,-40.9486306677112,-0.30801769742773));
#8694=CARTESIAN_POINT('Ctrl Pts',(16.5615744836782,-41.1374255872483,-0.0281983728666175));
#8695=CARTESIAN_POINT('Ctrl Pts',(16.6631435194004,-41.3262205067854,0.251620951694495));
#8696=CARTESIAN_POINT('Ctrl Pts',(16.8704078626898,-41.4539922120466,0.506521968549832));
#8697=CARTESIAN_POINT('Ctrl Pts',(17.0776722059792,-41.5817639173077,0.761422985405168));
#8698=CARTESIAN_POINT('Ctrl Pts',(17.370801568595,-41.6599614305468,0.940919422010711));
#8699=CARTESIAN_POINT('Ctrl Pts',(17.6639309312109,-41.7381589437859,1.12041585861625));
#8700=CARTESIAN_POINT('Ctrl Pts',(18.0060884047694,-41.7880500639744,1.18895624432295));
#8701=CARTESIAN_POINT('Ctrl Pts',(18.3482458783279,-41.8379411841628,1.25749663002964));
#8702=CARTESIAN_POINT('Ctrl Pts',(18.6928839357828,-41.8864001385709,1.2015057008556));
#8703=CARTESIAN_POINT('Ctrl Pts',(19.0375219932377,-41.934859092979,1.14551477168157));
#8704=CARTESIAN_POINT('Ctrl Pts',(19.3376017974798,-42.0090437668742,0.976082217833403));
#8705=CARTESIAN_POINT('Ctrl Pts',(19.6376816017219,-42.0832284407693,0.80664966398524));
#8706=CARTESIAN_POINT('Ctrl Pts',(19.8549896241618,-42.2052014251693,0.557333680706485));
#8707=CARTESIAN_POINT('Ctrl Pts',(20.0722976466017,-42.3271744095693,0.308017697427731));
#8708=CARTESIAN_POINT('Ctrl Pts',(20.1850143251651,-42.5095332345112,0.0281983728666177));
#8709=CARTESIAN_POINT('Ctrl Pts',(20.2977310037286,-42.6918920594531,-0.251620951694495));
#8710=CARTESIAN_POINT('Ctrl Pts',(20.3047523747249,-42.935274098671,-0.506521968549832));
#8711=CARTESIAN_POINT('Ctrl Pts',(20.3117737457212,-43.1786561378889,-0.761422985405168));
#8712=CARTESIAN_POINT('Ctrl Pts',(20.2329300973911,-43.4716123691288,-0.940919422010711));
#8713=CARTESIAN_POINT('Ctrl Pts',(20.154086449061,-43.7645686003688,-1.12041585861625));
#8714=CARTESIAN_POINT('Ctrl Pts',(20.0262146897883,-44.0858312246594,-1.18895624432295));
#8715=CARTESIAN_POINT('Ctrl Pts',(19.8983429305155,-44.40709384895,-1.25749663002964));
#8716=CARTESIAN_POINT('Ctrl Pts',(19.7679905873462,-44.7297886390209,-1.2015057008556));
#8717=CARTESIAN_POINT('Ctrl Pts',(19.637638244177,-45.0524834290919,-1.14551477168157));
#8718=CARTESIAN_POINT('Ctrl Pts',(19.5518441542206,-45.3494524996758,-0.976082217833403));
#8719=CARTESIAN_POINT('Ctrl Pts',(3.62216201968442,-19.1056780894973,-1.2339885196899));
#8720=CARTESIAN_POINT('Ctrl Pts',(3.48538897159447,-19.4320798752826,-0.910806095028249));
#8721=CARTESIAN_POINT('Ctrl Pts',(3.49420839053257,-19.6744238110373,-0.497425511654571));
#8722=CARTESIAN_POINT('Ctrl Pts',(3.50302780947066,-19.916767746792,-0.0840449282808927));
#8723=CARTESIAN_POINT('Ctrl Pts',(3.67691385823109,-20.0638104193845,0.337658719487502));
#8724=CARTESIAN_POINT('Ctrl Pts',(3.85079990699151,-20.2108530919771,0.759362367255897));
#8725=CARTESIAN_POINT('Ctrl Pts',(4.17653327792288,-20.2702266722385,1.10586550012264));
#8726=CARTESIAN_POINT('Ctrl Pts',(4.50226664885425,-20.3296002524999,1.45236863298939));
#8727=CARTESIAN_POINT('Ctrl Pts',(4.93655280986403,-20.3263008501883,1.65504205590818));
#8728=CARTESIAN_POINT('Ctrl Pts',(5.3708389708738,-20.3230014478767,1.85771547882697));
#8729=CARTESIAN_POINT('Ctrl Pts',(5.84888317848182,-20.2944383255823,1.87641723476232));
#8730=CARTESIAN_POINT('Ctrl Pts',(6.32692738608983,-20.265875203288,1.89511899069768));
#8731=CARTESIAN_POINT('Ctrl Pts',(6.77526807902992,-20.2544614131831,1.72614496752462));
#8732=CARTESIAN_POINT('Ctrl Pts',(7.22360877197,-20.2430476230782,1.55717094435156));
#8733=CARTESIAN_POINT('Ctrl Pts',(7.57466753434566,-20.2877995817719,1.2339885196899));
#8734=CARTESIAN_POINT('Ctrl Pts',(7.92572629672132,-20.3325515404656,0.910806095028249));
#8735=CARTESIAN_POINT('Ctrl Pts',(8.13119259206894,-20.46136134919,0.497425511654571));
#8736=CARTESIAN_POINT('Ctrl Pts',(8.33665888741656,-20.5901711579143,0.084044928280893));
#8737=CARTESIAN_POINT('Ctrl Pts',(8.37705855294184,-20.8142822298008,-0.337658719487502));
#8738=CARTESIAN_POINT('Ctrl Pts',(8.41745821846713,-21.0383933016873,-0.759362367255897));
#8739=CARTESIAN_POINT('Ctrl Pts',(8.30601056182147,-21.350173465905,-1.10586550012264));
#8740=CARTESIAN_POINT('Ctrl Pts',(8.19456290517582,-21.6619536301226,-1.45236863298939));
#8741=CARTESIAN_POINT('Ctrl Pts',(7.97456245845175,-22.0364067769132,-1.65504205590818));
#8742=CARTESIAN_POINT('Ctrl Pts',(7.75456201172769,-22.4108599237039,-1.85771547882697));
#8743=CARTESIAN_POINT('Ctrl Pts',(7.49080351840538,-22.8105767904773,-1.87641723476232));
#8744=CARTESIAN_POINT('Ctrl Pts',(7.22704502508308,-23.2102936572507,-1.89511899069768));
#8745=CARTESIAN_POINT('Ctrl Pts',(6.99299004642871,-23.5928611918346,-1.72614496752462));
#8746=CARTESIAN_POINT('Ctrl Pts',(6.75893506777434,-23.9754287264186,-1.55717094435156));
#8747=CARTESIAN_POINT('Ctrl Pts',(6.62216201968439,-24.3018305122039,-1.2339885196899));
#8748=CARTESIAN_POINT('Ctrl Pts',(6.48538897159444,-24.6282322979892,-0.910806095028249));
#8749=CARTESIAN_POINT('Ctrl Pts',(6.49420839053254,-24.8705762337439,-0.497425511654571));
#8750=CARTESIAN_POINT('Ctrl Pts',(6.50302780947063,-25.1129201694986,-0.0840449282808927));
#8751=CARTESIAN_POINT('Ctrl Pts',(6.67691385823105,-25.2599628420912,0.337658719487502));
#8752=CARTESIAN_POINT('Ctrl Pts',(6.85079990699148,-25.4070055146837,0.759362367255897));
#8753=CARTESIAN_POINT('Ctrl Pts',(7.17653327792285,-25.4663790949451,1.10586550012264));
#8754=CARTESIAN_POINT('Ctrl Pts',(7.50226664885422,-25.5257526752066,1.45236863298939));
#8755=CARTESIAN_POINT('Ctrl Pts',(7.936552809864,-25.5224532728949,1.65504205590818));
#8756=CARTESIAN_POINT('Ctrl Pts',(8.37083897087377,-25.5191538705833,1.85771547882697));
#8757=CARTESIAN_POINT('Ctrl Pts',(8.84888317848179,-25.490590748289,1.87641723476232));
#8758=CARTESIAN_POINT('Ctrl Pts',(9.3269273860898,-25.4620276259946,1.89511899069768));
#8759=CARTESIAN_POINT('Ctrl Pts',(9.77526807902988,-25.4506138358897,1.72614496752462));
#8760=CARTESIAN_POINT('Ctrl Pts',(10.22360877197,-25.4392000457848,1.55717094435156));
#8761=CARTESIAN_POINT('Ctrl Pts',(10.5746675343456,-25.4839520044785,1.2339885196899));
#8762=CARTESIAN_POINT('Ctrl Pts',(10.9257262967213,-25.5287039631723,0.910806095028249));
#8763=CARTESIAN_POINT('Ctrl Pts',(11.1311925920689,-25.6575137718966,0.497425511654571));
#8764=CARTESIAN_POINT('Ctrl Pts',(11.3366588874165,-25.786323580621,0.084044928280893));
#8765=CARTESIAN_POINT('Ctrl Pts',(11.3770585529418,-26.0104346525075,-0.337658719487502));
#8766=CARTESIAN_POINT('Ctrl Pts',(11.4174582184671,-26.234545724394,-0.759362367255897));
#8767=CARTESIAN_POINT('Ctrl Pts',(11.3060105618214,-26.5463258886116,-1.10586550012264));
#8768=CARTESIAN_POINT('Ctrl Pts',(11.1945629051758,-26.8581060528292,-1.45236863298939));
#8769=CARTESIAN_POINT('Ctrl Pts',(10.9745624584517,-27.2325591996199,-1.65504205590818));
#8770=CARTESIAN_POINT('Ctrl Pts',(10.7545620117277,-27.6070123464106,-1.85771547882697));
#8771=CARTESIAN_POINT('Ctrl Pts',(10.4908035184054,-28.0067292131839,-1.87641723476232));
#8772=CARTESIAN_POINT('Ctrl Pts',(10.227045025083,-28.4064460799573,-1.89511899069768));
#8773=CARTESIAN_POINT('Ctrl Pts',(9.99299004642868,-28.7890136145413,-1.72614496752462));
#8774=CARTESIAN_POINT('Ctrl Pts',(9.75893506777431,-29.1715811491253,-1.55717094435156));
#8775=CARTESIAN_POINT('Ctrl Pts',(9.62216201968436,-29.4979829349106,-1.2339885196899));
#8776=CARTESIAN_POINT('Ctrl Pts',(9.48538897159441,-29.8243847206959,-0.910806095028249));
#8777=CARTESIAN_POINT('Ctrl Pts',(9.4942083905325,-30.0667286564506,-0.497425511654571));
#8778=CARTESIAN_POINT('Ctrl Pts',(9.5030278094706,-30.3090725922053,-0.0840449282808927));
#8779=CARTESIAN_POINT('Ctrl Pts',(9.67691385823102,-30.4561152647978,0.337658719487502));
#8780=CARTESIAN_POINT('Ctrl Pts',(9.85079990699145,-30.6031579373903,0.759362367255897));
#8781=CARTESIAN_POINT('Ctrl Pts',(10.1765332779228,-30.6625315176518,1.10586550012264));
#8782=CARTESIAN_POINT('Ctrl Pts',(10.5022666488542,-30.7219050979132,1.45236863298939));
#8783=CARTESIAN_POINT('Ctrl Pts',(10.936552809864,-30.7186056956016,1.65504205590818));
#8784=CARTESIAN_POINT('Ctrl Pts',(11.3708389708737,-30.71530629329,1.85771547882697));
#8785=CARTESIAN_POINT('Ctrl Pts',(11.8488831784818,-30.6867431709956,1.87641723476232));
#8786=CARTESIAN_POINT('Ctrl Pts',(12.3269273860898,-30.6581800487013,1.89511899069768));
#8787=CARTESIAN_POINT('Ctrl Pts',(12.7752680790299,-30.6467662585964,1.72614496752462));
#8788=CARTESIAN_POINT('Ctrl Pts',(13.2236087719699,-30.6353524684915,1.55717094435156));
#8789=CARTESIAN_POINT('Ctrl Pts',(13.5746675343456,-30.6801044271852,1.2339885196899));
#8790=CARTESIAN_POINT('Ctrl Pts',(13.9257262967213,-30.7248563858789,0.910806095028249));
#8791=CARTESIAN_POINT('Ctrl Pts',(14.1311925920689,-30.8536661946033,0.497425511654571));
#8792=CARTESIAN_POINT('Ctrl Pts',(14.3366588874165,-30.9824760033276,0.084044928280893));
#8793=CARTESIAN_POINT('Ctrl Pts',(14.3770585529418,-31.2065870752141,-0.337658719487502));
#8794=CARTESIAN_POINT('Ctrl Pts',(14.4174582184671,-31.4306981471006,-0.759362367255897));
#8795=CARTESIAN_POINT('Ctrl Pts',(14.3060105618214,-31.7424783113183,-1.10586550012264));
#8796=CARTESIAN_POINT('Ctrl Pts',(14.1945629051758,-32.0542584755359,-1.45236863298939));
#8797=CARTESIAN_POINT('Ctrl Pts',(13.9745624584517,-32.4287116223265,-1.65504205590818));
#8798=CARTESIAN_POINT('Ctrl Pts',(13.7545620117276,-32.8031647691172,-1.85771547882697));
#8799=CARTESIAN_POINT('Ctrl Pts',(13.4908035184053,-33.2028816358906,-1.87641723476232));
#8800=CARTESIAN_POINT('Ctrl Pts',(13.227045025083,-33.602598502664,-1.89511899069768));
#8801=CARTESIAN_POINT('Ctrl Pts',(12.9929900464286,-33.9851660372479,-1.72614496752462));
#8802=CARTESIAN_POINT('Ctrl Pts',(12.7589350677743,-34.3677335718319,-1.55717094435156));
#8803=CARTESIAN_POINT('Ctrl Pts',(12.6221620196843,-34.6941353576172,-1.2339885196899));
#8804=CARTESIAN_POINT('Ctrl Pts',(12.4853889715944,-35.0205371434025,-0.910806095028249));
#8805=CARTESIAN_POINT('Ctrl Pts',(12.4942083905325,-35.2628810791572,-0.497425511654571));
#8806=CARTESIAN_POINT('Ctrl Pts',(12.5030278094706,-35.5052250149119,-0.0840449282808927));
#8807=CARTESIAN_POINT('Ctrl Pts',(12.676913858231,-35.6522676875044,0.337658719487502));
#8808=CARTESIAN_POINT('Ctrl Pts',(12.8507999069914,-35.799310360097,0.759362367255897));
#8809=CARTESIAN_POINT('Ctrl Pts',(13.1765332779228,-35.8586839403584,1.10586550012264));
#8810=CARTESIAN_POINT('Ctrl Pts',(13.5022666488542,-35.9180575206199,1.45236863298939));
#8811=CARTESIAN_POINT('Ctrl Pts',(13.9365528098639,-35.9147581183082,1.65504205590818));
#8812=CARTESIAN_POINT('Ctrl Pts',(14.3708389708737,-35.9114587159966,1.85771547882697));
#8813=CARTESIAN_POINT('Ctrl Pts',(14.8488831784817,-35.8828955937023,1.87641723476232));
#8814=CARTESIAN_POINT('Ctrl Pts',(15.3269273860897,-35.8543324714079,1.89511899069768));
#8815=CARTESIAN_POINT('Ctrl Pts',(15.7752680790298,-35.842918681303,1.72614496752462));
#8816=CARTESIAN_POINT('Ctrl Pts',(16.2236087719699,-35.8315048911981,1.55717094435156));
#8817=CARTESIAN_POINT('Ctrl Pts',(16.5746675343456,-35.8762568498918,1.2339885196899));
#8818=CARTESIAN_POINT('Ctrl Pts',(16.9257262967212,-35.9210088085856,0.910806095028249));
#8819=CARTESIAN_POINT('Ctrl Pts',(17.1311925920688,-36.0498186173099,0.497425511654571));
#8820=CARTESIAN_POINT('Ctrl Pts',(17.3366588874165,-36.1786284260343,0.084044928280893));
#8821=CARTESIAN_POINT('Ctrl Pts',(17.3770585529417,-36.4027394979208,-0.337658719487502));
#8822=CARTESIAN_POINT('Ctrl Pts',(17.417458218467,-36.6268505698073,-0.759362367255897));
#8823=CARTESIAN_POINT('Ctrl Pts',(17.3060105618214,-36.9386307340249,-1.10586550012264));
#8824=CARTESIAN_POINT('Ctrl Pts',(17.1945629051757,-37.2504108982425,-1.45236863298939));
#8825=CARTESIAN_POINT('Ctrl Pts',(16.9745624584517,-37.6248640450332,-1.65504205590818));
#8826=CARTESIAN_POINT('Ctrl Pts',(16.7545620117276,-37.9993171918239,-1.85771547882697));
#8827=CARTESIAN_POINT('Ctrl Pts',(16.4908035184053,-38.3990340585972,-1.87641723476232));
#8828=CARTESIAN_POINT('Ctrl Pts',(16.227045025083,-38.7987509253706,-1.89511899069768));
#8829=CARTESIAN_POINT('Ctrl Pts',(15.9929900464286,-39.1813184599546,-1.72614496752462));
#8830=CARTESIAN_POINT('Ctrl Pts',(15.7589350677742,-39.5638859945386,-1.55717094435156));
#8831=CARTESIAN_POINT('Ctrl Pts',(15.6221620196843,-39.8902877803239,-1.2339885196899));
#8832=CARTESIAN_POINT('Ctrl Pts',(15.4853889715943,-40.2166895661092,-0.910806095028249));
#8833=CARTESIAN_POINT('Ctrl Pts',(15.4942083905324,-40.4590335018639,-0.497425511654571));
#8834=CARTESIAN_POINT('Ctrl Pts',(15.5030278094705,-40.7013774376186,-0.0840449282808927));
#8835=CARTESIAN_POINT('Ctrl Pts',(15.676913858231,-40.8484201102111,0.337658719487502));
#8836=CARTESIAN_POINT('Ctrl Pts',(15.8507999069914,-40.9954627828037,0.759362367255897));
#8837=CARTESIAN_POINT('Ctrl Pts',(16.1765332779228,-41.0548363630651,1.10586550012264));
#8838=CARTESIAN_POINT('Ctrl Pts',(16.5022666488541,-41.1142099433265,1.45236863298939));
#8839=CARTESIAN_POINT('Ctrl Pts',(16.9365528098639,-41.1109105410149,1.65504205590818));
#8840=CARTESIAN_POINT('Ctrl Pts',(17.3708389708737,-41.1076111387033,1.85771547882697));
#8841=CARTESIAN_POINT('Ctrl Pts',(17.8488831784817,-41.0790480164089,1.87641723476232));
#8842=CARTESIAN_POINT('Ctrl Pts',(18.3269273860897,-41.0504848941146,1.89511899069768));
#8843=CARTESIAN_POINT('Ctrl Pts',(18.7752680790298,-41.0390711040097,1.72614496752462));
#8844=CARTESIAN_POINT('Ctrl Pts',(19.2236087719699,-41.0276573139048,1.55717094435156));
#8845=CARTESIAN_POINT('Ctrl Pts',(19.5746675343455,-41.0724092725985,1.2339885196899));
#8846=CARTESIAN_POINT('Ctrl Pts',(19.9257262967212,-41.1171612312922,0.910806095028249));
#8847=CARTESIAN_POINT('Ctrl Pts',(20.1311925920688,-41.2459710400166,0.497425511654571));
#8848=CARTESIAN_POINT('Ctrl Pts',(20.3366588874164,-41.374780848741,0.084044928280893));
#8849=CARTESIAN_POINT('Ctrl Pts',(20.3770585529417,-41.5988919206274,-0.337658719487502));
#8850=CARTESIAN_POINT('Ctrl Pts',(20.417458218467,-41.823002992514,-0.759362367255897));
#8851=CARTESIAN_POINT('Ctrl Pts',(20.3060105618213,-42.1347831567316,-1.10586550012264));
#8852=CARTESIAN_POINT('Ctrl Pts',(20.1945629051757,-42.4465633209492,-1.45236863298939));
#8853=CARTESIAN_POINT('Ctrl Pts',(19.9745624584516,-42.8210164677398,-1.65504205590818));
#8854=CARTESIAN_POINT('Ctrl Pts',(19.7545620117276,-43.1954696145305,-1.85771547882697));
#8855=CARTESIAN_POINT('Ctrl Pts',(19.4908035184053,-43.5951864813039,-1.87641723476232));
#8856=CARTESIAN_POINT('Ctrl Pts',(19.227045025083,-43.9949033480773,-1.89511899069768));
#8857=CARTESIAN_POINT('Ctrl Pts',(18.9929900464286,-44.3774708826612,-1.72614496752462));
#8858=CARTESIAN_POINT('Ctrl Pts',(18.7589350677742,-44.7600384172452,-1.55717094435156));
#8859=CARTESIAN_POINT('Ctrl Pts',(18.6221620196843,-45.0864402030305,-1.2339885196899));
#8860=CARTESIAN_POINT('Ctrl Pts',(2.69247988514806,-18.842665792852,-1.4918948215464));
#8861=CARTESIAN_POINT('Ctrl Pts',(2.50472787892454,-19.1985002938387,-1.01496252607126));
#8862=CARTESIAN_POINT('Ctrl Pts',(2.52538902495489,-19.434007405269,-0.437517342602656));
#8863=CARTESIAN_POINT('Ctrl Pts',(2.54605017098523,-19.6695145166993,0.139927840865946));
#8864=CARTESIAN_POINT('Ctrl Pts',(2.79225323278385,-19.7748049423473,0.703515811841622));
#8865=CARTESIAN_POINT('Ctrl Pts',(3.03845629458247,-19.8800953679953,1.2671037828173));
#8866=CARTESIAN_POINT('Ctrl Pts',(3.48265869315581,-19.871070823257,1.70520903169545));
#8867=CARTESIAN_POINT('Ctrl Pts',(3.92686109172914,-19.8620462785187,2.1433142805736));
#8868=CARTESIAN_POINT('Ctrl Pts',(4.50230405113288,-19.7772499606563,2.36916468980564));
#8869=CARTESIAN_POINT('Ctrl Pts',(5.07774701053662,-19.692453642794,2.59501509903768));
#8870=CARTESIAN_POINT('Ctrl Pts',(5.69167795219416,-19.5854362780169,2.5638782252017));
#8871=CARTESIAN_POINT('Ctrl Pts',(6.30560889385169,-19.4784189132398,2.53274135136572));
#8872=CARTESIAN_POINT('Ctrl Pts',(6.85765222227691,-19.4071323786218,2.25078423419363));
#8873=CARTESIAN_POINT('Ctrl Pts',(7.40969555070213,-19.3358458440039,1.96882711702155));
#8874=CARTESIAN_POINT('Ctrl Pts',(7.81173327121136,-19.3511650874962,1.4918948215464));
#8875=CARTESIAN_POINT('Ctrl Pts',(8.21377099172059,-19.3664843309885,1.01496252607126));
#8876=CARTESIAN_POINT('Ctrl Pts',(8.40739555997595,-19.5021309640373,0.437517342602656));
#8877=CARTESIAN_POINT('Ctrl Pts',(8.60102012823132,-19.637777597086,-0.139927840865945));
#8878=CARTESIAN_POINT('Ctrl Pts',(8.56910278071841,-19.9036409159171,-0.703515811841622));
#8879=CARTESIAN_POINT('Ctrl Pts',(8.5371854332055,-20.1695042347482,-1.2671037828173));
#8880=CARTESIAN_POINT('Ctrl Pts',(8.30726874891788,-20.5496825239655,-1.70520903169545));
#8881=CARTESIAN_POINT('Ctrl Pts',(8.07735206463027,-20.9298608131829,-2.1433142805736));
#8882=CARTESIAN_POINT('Ctrl Pts',(7.71619481951224,-21.3858108755242,-2.36916468980564));
#8883=CARTESIAN_POINT('Ctrl Pts',(7.35503757439421,-21.8417609378656,-2.59501509903768));
#8884=CARTESIAN_POINT('Ctrl Pts',(6.95539234702238,-22.3199320471218,-2.5638782252017));
#8885=CARTESIAN_POINT('Ctrl Pts',(6.55574711965056,-22.7981031563779,-2.53274135136572));
#8886=CARTESIAN_POINT('Ctrl Pts',(6.21798950551105,-23.2405434354749,-2.25078423419363));
#8887=CARTESIAN_POINT('Ctrl Pts',(5.88023189137154,-23.6829837145719,-1.96882711702155));
#8888=CARTESIAN_POINT('Ctrl Pts',(5.69247988514803,-24.0388182155586,-1.4918948215464));
#8889=CARTESIAN_POINT('Ctrl Pts',(5.50472787892451,-24.3946527165454,-1.01496252607126));
#8890=CARTESIAN_POINT('Ctrl Pts',(5.52538902495486,-24.6301598279757,-0.437517342602656));
#8891=CARTESIAN_POINT('Ctrl Pts',(5.5460501709852,-24.865666939406,0.139927840865946));
#8892=CARTESIAN_POINT('Ctrl Pts',(5.79225323278382,-24.970957365054,0.703515811841622));
#8893=CARTESIAN_POINT('Ctrl Pts',(6.03845629458244,-25.0762477907019,1.2671037828173));
#8894=CARTESIAN_POINT('Ctrl Pts',(6.48265869315577,-25.0672232459636,1.70520903169545));
#8895=CARTESIAN_POINT('Ctrl Pts',(6.92686109172911,-25.0581987012253,2.1433142805736));
#8896=CARTESIAN_POINT('Ctrl Pts',(7.50230405113285,-24.973402383363,2.36916468980564));
#8897=CARTESIAN_POINT('Ctrl Pts',(8.07774701053659,-24.8886060655007,2.59501509903768));
#8898=CARTESIAN_POINT('Ctrl Pts',(8.69167795219413,-24.7815887007236,2.5638782252017));
#8899=CARTESIAN_POINT('Ctrl Pts',(9.30560889385166,-24.6745713359464,2.53274135136572));
#8900=CARTESIAN_POINT('Ctrl Pts',(9.85765222227688,-24.6032848013285,2.25078423419363));
#8901=CARTESIAN_POINT('Ctrl Pts',(10.4096955507021,-24.5319982667106,1.96882711702155));
#8902=CARTESIAN_POINT('Ctrl Pts',(10.8117332712113,-24.5473175102029,1.4918948215464));
#8903=CARTESIAN_POINT('Ctrl Pts',(11.2137709917206,-24.5626367536952,1.01496252607126));
#8904=CARTESIAN_POINT('Ctrl Pts',(11.4073955599759,-24.6982833867439,0.437517342602656));
#8905=CARTESIAN_POINT('Ctrl Pts',(11.6010201282313,-24.8339300197927,-0.139927840865945));
#8906=CARTESIAN_POINT('Ctrl Pts',(11.5691027807184,-25.0997933386238,-0.703515811841622));
#8907=CARTESIAN_POINT('Ctrl Pts',(11.5371854332055,-25.3656566574548,-1.2671037828173));
#8908=CARTESIAN_POINT('Ctrl Pts',(11.3072687489179,-25.7458349466722,-1.70520903169545));
#8909=CARTESIAN_POINT('Ctrl Pts',(11.0773520646302,-26.1260132358895,-2.1433142805736));
#8910=CARTESIAN_POINT('Ctrl Pts',(10.7161948195122,-26.5819632982309,-2.36916468980564));
#8911=CARTESIAN_POINT('Ctrl Pts',(10.3550375743942,-27.0379133605723,-2.59501509903768));
#8912=CARTESIAN_POINT('Ctrl Pts',(9.95539234702235,-27.5160844698284,-2.5638782252017));
#8913=CARTESIAN_POINT('Ctrl Pts',(9.55574711965053,-27.9942555790846,-2.53274135136572));
#8914=CARTESIAN_POINT('Ctrl Pts',(9.21798950551102,-28.4366958581816,-2.25078423419363));
#8915=CARTESIAN_POINT('Ctrl Pts',(8.88023189137151,-28.8791361372786,-1.96882711702155));
#8916=CARTESIAN_POINT('Ctrl Pts',(8.692479885148,-29.2349706382653,-1.4918948215464));
#8917=CARTESIAN_POINT('Ctrl Pts',(8.50472787892448,-29.590805139252,-1.01496252607126));
#8918=CARTESIAN_POINT('Ctrl Pts',(8.52538902495483,-29.8263122506823,-0.437517342602656));
#8919=CARTESIAN_POINT('Ctrl Pts',(8.54605017098517,-30.0618193621126,0.139927840865946));
#8920=CARTESIAN_POINT('Ctrl Pts',(8.79225323278379,-30.1671097877606,0.703515811841622));
#8921=CARTESIAN_POINT('Ctrl Pts',(9.03845629458241,-30.2724002134086,1.2671037828173));
#8922=CARTESIAN_POINT('Ctrl Pts',(9.48265869315574,-30.2633756686703,1.70520903169545));
#8923=CARTESIAN_POINT('Ctrl Pts',(9.92686109172908,-30.254351123932,2.1433142805736));
#8924=CARTESIAN_POINT('Ctrl Pts',(10.5023040511328,-30.1695548060697,2.36916468980564));
#8925=CARTESIAN_POINT('Ctrl Pts',(11.0777470105366,-30.0847584882073,2.59501509903768));
#8926=CARTESIAN_POINT('Ctrl Pts',(11.6916779521941,-29.9777411234302,2.5638782252017));
#8927=CARTESIAN_POINT('Ctrl Pts',(12.3056088938516,-29.8707237586531,2.53274135136572));
#8928=CARTESIAN_POINT('Ctrl Pts',(12.8576522222768,-29.7994372240352,2.25078423419363));
#8929=CARTESIAN_POINT('Ctrl Pts',(13.4096955507021,-29.7281506894172,1.96882711702155));
#8930=CARTESIAN_POINT('Ctrl Pts',(13.8117332712113,-29.7434699329095,1.4918948215464));
#8931=CARTESIAN_POINT('Ctrl Pts',(14.2137709917205,-29.7587891764018,1.01496252607126));
#8932=CARTESIAN_POINT('Ctrl Pts',(14.4073955599759,-29.8944358094506,0.437517342602656));
#8933=CARTESIAN_POINT('Ctrl Pts',(14.6010201282313,-30.0300824424993,-0.139927840865945));
#8934=CARTESIAN_POINT('Ctrl Pts',(14.5691027807183,-30.2959457613304,-0.703515811841622));
#8935=CARTESIAN_POINT('Ctrl Pts',(14.5371854332054,-30.5618090801615,-1.2671037828173));
#8936=CARTESIAN_POINT('Ctrl Pts',(14.3072687489178,-30.9419873693788,-1.70520903169545));
#8937=CARTESIAN_POINT('Ctrl Pts',(14.0773520646302,-31.3221656585962,-2.1433142805736));
#8938=CARTESIAN_POINT('Ctrl Pts',(13.7161948195122,-31.7781157209375,-2.36916468980564));
#8939=CARTESIAN_POINT('Ctrl Pts',(13.3550375743941,-32.2340657832789,-2.59501509903768));
#8940=CARTESIAN_POINT('Ctrl Pts',(12.9553923470223,-32.7122368925351,-2.5638782252017));
#8941=CARTESIAN_POINT('Ctrl Pts',(12.5557471196505,-33.1904080017912,-2.53274135136572));
#8942=CARTESIAN_POINT('Ctrl Pts',(12.217989505511,-33.6328482808882,-2.25078423419363));
#8943=CARTESIAN_POINT('Ctrl Pts',(11.8802318913715,-34.0752885599852,-1.96882711702155));
#8944=CARTESIAN_POINT('Ctrl Pts',(11.692479885148,-34.4311230609719,-1.4918948215464));
#8945=CARTESIAN_POINT('Ctrl Pts',(11.5047278789244,-34.7869575619587,-1.01496252607126));
#8946=CARTESIAN_POINT('Ctrl Pts',(11.5253890249548,-35.022464673389,-0.437517342602656));
#8947=CARTESIAN_POINT('Ctrl Pts',(11.5460501709851,-35.2579717848193,0.139927840865946));
#8948=CARTESIAN_POINT('Ctrl Pts',(11.7922532327838,-35.3632622104672,0.703515811841622));
#8949=CARTESIAN_POINT('Ctrl Pts',(12.0384562945824,-35.4685526361152,1.2671037828173));
#8950=CARTESIAN_POINT('Ctrl Pts',(12.4826586931557,-35.4595280913769,1.70520903169545));
#8951=CARTESIAN_POINT('Ctrl Pts',(12.926861091729,-35.4505035466386,2.1433142805736));
#8952=CARTESIAN_POINT('Ctrl Pts',(13.5023040511328,-35.3657072287763,2.36916468980564));
#8953=CARTESIAN_POINT('Ctrl Pts',(14.0777470105365,-35.280910910914,2.59501509903768));
#8954=CARTESIAN_POINT('Ctrl Pts',(14.6916779521941,-35.1738935461369,2.5638782252017));
#8955=CARTESIAN_POINT('Ctrl Pts',(15.3056088938516,-35.0668761813597,2.53274135136572));
#8956=CARTESIAN_POINT('Ctrl Pts',(15.8576522222768,-34.9955896467418,2.25078423419363));
#8957=CARTESIAN_POINT('Ctrl Pts',(16.409695550702,-34.9243031121239,1.96882711702155));
#8958=CARTESIAN_POINT('Ctrl Pts',(16.8117332712113,-34.9396223556162,1.4918948215464));
#8959=CARTESIAN_POINT('Ctrl Pts',(17.2137709917205,-34.9549415991085,1.01496252607126));
#8960=CARTESIAN_POINT('Ctrl Pts',(17.4073955599759,-35.0905882321572,0.437517342602656));
#8961=CARTESIAN_POINT('Ctrl Pts',(17.6010201282312,-35.226234865206,-0.139927840865945));
#8962=CARTESIAN_POINT('Ctrl Pts',(17.5691027807183,-35.4920981840371,-0.703515811841622));
#8963=CARTESIAN_POINT('Ctrl Pts',(17.5371854332054,-35.7579615028681,-1.2671037828173));
#8964=CARTESIAN_POINT('Ctrl Pts',(17.3072687489178,-36.1381397920855,-1.70520903169545));
#8965=CARTESIAN_POINT('Ctrl Pts',(17.0773520646302,-36.5183180813028,-2.1433142805736));
#8966=CARTESIAN_POINT('Ctrl Pts',(16.7161948195121,-36.9742681436442,-2.36916468980564));
#8967=CARTESIAN_POINT('Ctrl Pts',(16.3550375743941,-37.4302182059856,-2.59501509903768));
#8968=CARTESIAN_POINT('Ctrl Pts',(15.9553923470223,-37.9083893152417,-2.5638782252017));
#8969=CARTESIAN_POINT('Ctrl Pts',(15.5557471196505,-38.3865604244979,-2.53274135136572));
#8970=CARTESIAN_POINT('Ctrl Pts',(15.217989505511,-38.8290007035949,-2.25078423419363));
#8971=CARTESIAN_POINT('Ctrl Pts',(14.8802318913715,-39.2714409826919,-1.96882711702155));
#8972=CARTESIAN_POINT('Ctrl Pts',(14.6924798851479,-39.6272754836786,-1.4918948215464));
#8973=CARTESIAN_POINT('Ctrl Pts',(14.5047278789244,-39.9831099846653,-1.01496252607126));
#8974=CARTESIAN_POINT('Ctrl Pts',(14.5253890249548,-40.2186170960956,-0.437517342602656));
#8975=CARTESIAN_POINT('Ctrl Pts',(14.5460501709851,-40.4541242075259,0.139927840865946));
#8976=CARTESIAN_POINT('Ctrl Pts',(14.7922532327837,-40.5594146331739,0.703515811841622));
#8977=CARTESIAN_POINT('Ctrl Pts',(15.0384562945823,-40.6647050588219,1.2671037828173));
#8978=CARTESIAN_POINT('Ctrl Pts',(15.4826586931557,-40.6556805140836,1.70520903169545));
#8979=CARTESIAN_POINT('Ctrl Pts',(15.926861091729,-40.6466559693453,2.1433142805736));
#8980=CARTESIAN_POINT('Ctrl Pts',(16.5023040511328,-40.5618596514829,2.36916468980564));
#8981=CARTESIAN_POINT('Ctrl Pts',(17.0777470105365,-40.4770633336206,2.59501509903768));
#8982=CARTESIAN_POINT('Ctrl Pts',(17.691677952194,-40.3700459688435,2.5638782252017));
#8983=CARTESIAN_POINT('Ctrl Pts',(18.3056088938516,-40.2630286040664,2.53274135136572));
#8984=CARTESIAN_POINT('Ctrl Pts',(18.8576522222768,-40.1917420694485,2.25078423419363));
#8985=CARTESIAN_POINT('Ctrl Pts',(19.409695550702,-40.1204555348305,1.96882711702155));
#8986=CARTESIAN_POINT('Ctrl Pts',(19.8117332712112,-40.1357747783228,1.4918948215464));
#8987=CARTESIAN_POINT('Ctrl Pts',(20.2137709917205,-40.1510940218152,1.01496252607126));
#8988=CARTESIAN_POINT('Ctrl Pts',(20.4073955599758,-40.2867406548639,0.437517342602656));
#8989=CARTESIAN_POINT('Ctrl Pts',(20.6010201282312,-40.4223872879126,-0.139927840865945));
#8990=CARTESIAN_POINT('Ctrl Pts',(20.5691027807183,-40.6882506067437,-0.703515811841622));
#8991=CARTESIAN_POINT('Ctrl Pts',(20.5371854332054,-40.9541139255748,-1.2671037828173));
#8992=CARTESIAN_POINT('Ctrl Pts',(20.3072687489178,-41.3342922147921,-1.70520903169545));
#8993=CARTESIAN_POINT('Ctrl Pts',(20.0773520646301,-41.7144705040095,-2.1433142805736));
#8994=CARTESIAN_POINT('Ctrl Pts',(19.7161948195121,-42.1704205663508,-2.36916468980564));
#8995=CARTESIAN_POINT('Ctrl Pts',(19.3550375743941,-42.6263706286922,-2.59501509903768));
#8996=CARTESIAN_POINT('Ctrl Pts',(18.9553923470223,-43.1045417379484,-2.5638782252017));
#8997=CARTESIAN_POINT('Ctrl Pts',(18.5557471196504,-43.5827128472045,-2.53274135136572));
#8998=CARTESIAN_POINT('Ctrl Pts',(18.2179895055109,-44.0251531263015,-2.25078423419363));
#8999=CARTESIAN_POINT('Ctrl Pts',(17.8802318913714,-44.4675934053985,-1.96882711702155));
#9000=CARTESIAN_POINT('Ctrl Pts',(17.6924798851479,-44.8234279063853,-1.4918948215464));
#9001=CARTESIAN_POINT('Ctrl Pts',(2.69247988514806,-19.542807947216,-2.20589829750609));
#9002=CARTESIAN_POINT('Ctrl Pts',(2.3635946338423,-19.9801257652426,-1.64906456309142));
#9003=CARTESIAN_POINT('Ctrl Pts',(2.28712243231041,-20.2717128410352,-0.928922098091803));
#9004=CARTESIAN_POINT('Ctrl Pts',(2.21065023077853,-20.5632999168279,-0.208779633092189));
#9005=CARTESIAN_POINT('Ctrl Pts',(2.42295829328197,-20.6881596294431,0.532038515331462));
#9006=CARTESIAN_POINT('Ctrl Pts',(2.63526635578541,-20.8130193420583,1.27285666375511));
#9007=CARTESIAN_POINT('Ctrl Pts',(3.1155254236359,-20.7831774696068,1.88762237576914));
#9008=CARTESIAN_POINT('Ctrl Pts',(3.5957844914864,-20.7533355971552,2.50238808778318));
#9009=CARTESIAN_POINT('Ctrl Pts',(4.27009432318328,-20.6114584639605,2.86933947451654));
#9010=CARTESIAN_POINT('Ctrl Pts',(4.94440415488017,-20.4695813307658,3.2362908612499));
#9011=CARTESIAN_POINT('Ctrl Pts',(5.70043037526654,-20.280525218564,3.28274870019663));
#9012=CARTESIAN_POINT('Ctrl Pts',(6.45645659565292,-20.0914691063622,3.32920653914337));
#9013=CARTESIAN_POINT('Ctrl Pts',(7.1656798966062,-19.929434672294,3.04596928553206));
#9014=CARTESIAN_POINT('Ctrl Pts',(7.87490319755949,-19.7674002382258,2.76273203192075));
#9015=CARTESIAN_POINT('Ctrl Pts',(8.41807416315096,-19.7012361646782,2.20589829750609));
#9016=CARTESIAN_POINT('Ctrl Pts',(8.96124512874244,-19.6350720911307,1.64906456309142));
#9017=CARTESIAN_POINT('Ctrl Pts',(9.25200304456004,-19.7146387598171,0.928922098091803));
#9018=CARTESIAN_POINT('Ctrl Pts',(9.54276096037763,-19.7942054285035,0.20877963309219));
#9019=CARTESIAN_POINT('Ctrl Pts',(9.5447386121599,-20.0404994603673,-0.532038515331461));
#9020=CARTESIAN_POINT('Ctrl Pts',(9.54671626394218,-20.2867934922312,-1.27285666375511));
#9021=CARTESIAN_POINT('Ctrl Pts',(9.28074291037739,-20.6877891091618,-1.88762237576914));
#9022=CARTESIAN_POINT('Ctrl Pts',(9.01476955681261,-21.0887847260924,-2.50238808778318));
#9023=CARTESIAN_POINT('Ctrl Pts',(8.55474543940143,-21.6018156037661,-2.86933947451654));
#9024=CARTESIAN_POINT('Ctrl Pts',(8.09472132199027,-22.1148464814399,-3.2362908612499));
#9025=CARTESIAN_POINT('Ctrl Pts',(7.5529808158896,-22.6750563381207,-3.28274870019663));
#9026=CARTESIAN_POINT('Ctrl Pts',(7.01124030978894,-23.2352661948015,-3.32920653914337));
#9027=CARTESIAN_POINT('Ctrl Pts',(6.51630272312137,-23.7684543733488,-3.04596928553206));
#9028=CARTESIAN_POINT('Ctrl Pts',(6.02136513645379,-24.3016425518961,-2.76273203192075));
#9029=CARTESIAN_POINT('Ctrl Pts',(5.69247988514803,-24.7389603699227,-2.20589829750609));
#9030=CARTESIAN_POINT('Ctrl Pts',(5.36359463384226,-25.1762781879492,-1.64906456309142));
#9031=CARTESIAN_POINT('Ctrl Pts',(5.28712243231038,-25.4678652637419,-0.928922098091803));
#9032=CARTESIAN_POINT('Ctrl Pts',(5.2106502307785,-25.7594523395345,-0.208779633092189));
#9033=CARTESIAN_POINT('Ctrl Pts',(5.42295829328193,-25.8843120521498,0.532038515331462));
#9034=CARTESIAN_POINT('Ctrl Pts',(5.63526635578538,-26.009171764765,1.27285666375511));
#9035=CARTESIAN_POINT('Ctrl Pts',(6.11552542363587,-25.9793298923134,1.88762237576914));
#9036=CARTESIAN_POINT('Ctrl Pts',(6.59578449148637,-25.9494880198619,2.50238808778318));
#9037=CARTESIAN_POINT('Ctrl Pts',(7.27009432318325,-25.8076108866672,2.86933947451654));
#9038=CARTESIAN_POINT('Ctrl Pts',(7.94440415488013,-25.6657337534725,3.2362908612499));
#9039=CARTESIAN_POINT('Ctrl Pts',(8.70043037526651,-25.4766776412707,3.28274870019663));
#9040=CARTESIAN_POINT('Ctrl Pts',(9.45645659565288,-25.2876215290689,3.32920653914337));
#9041=CARTESIAN_POINT('Ctrl Pts',(10.1656798966062,-25.1255870950007,3.04596928553206));
#9042=CARTESIAN_POINT('Ctrl Pts',(10.8749031975595,-24.9635526609324,2.76273203192075));
#9043=CARTESIAN_POINT('Ctrl Pts',(11.4180741631509,-24.8973885873849,2.20589829750609));
#9044=CARTESIAN_POINT('Ctrl Pts',(11.9612451287424,-24.8312245138374,1.64906456309142));
#9045=CARTESIAN_POINT('Ctrl Pts',(12.25200304456,-24.9107911825238,0.928922098091803));
#9046=CARTESIAN_POINT('Ctrl Pts',(12.5427609603776,-24.9903578512102,0.20877963309219));
#9047=CARTESIAN_POINT('Ctrl Pts',(12.5447386121599,-25.236651883074,-0.532038515331461));
#9048=CARTESIAN_POINT('Ctrl Pts',(12.5467162639421,-25.4829459149378,-1.27285666375511));
#9049=CARTESIAN_POINT('Ctrl Pts',(12.2807429103774,-25.8839415318684,-1.88762237576914));
#9050=CARTESIAN_POINT('Ctrl Pts',(12.0147695568126,-26.284937148799,-2.50238808778318));
#9051=CARTESIAN_POINT('Ctrl Pts',(11.5547454394014,-26.7979680264728,-2.86933947451654));
#9052=CARTESIAN_POINT('Ctrl Pts',(11.0947213219902,-27.3109989041465,-3.2362908612499));
#9053=CARTESIAN_POINT('Ctrl Pts',(10.5529808158896,-27.8712087608274,-3.28274870019663));
#9054=CARTESIAN_POINT('Ctrl Pts',(10.0112403097889,-28.4314186175082,-3.32920653914337));
#9055=CARTESIAN_POINT('Ctrl Pts',(9.51630272312133,-28.9646067960555,-3.04596928553206));
#9056=CARTESIAN_POINT('Ctrl Pts',(9.02136513645376,-29.4977949746027,-2.76273203192075));
#9057=CARTESIAN_POINT('Ctrl Pts',(8.692479885148,-29.9351127926293,-2.20589829750609));
#9058=CARTESIAN_POINT('Ctrl Pts',(8.36359463384224,-30.3724306106559,-1.64906456309142));
#9059=CARTESIAN_POINT('Ctrl Pts',(8.28712243231035,-30.6640176864485,-0.928922098091803));
#9060=CARTESIAN_POINT('Ctrl Pts',(8.21065023077846,-30.9556047622412,-0.208779633092189));
#9061=CARTESIAN_POINT('Ctrl Pts',(8.4229582932819,-31.0804644748564,0.532038515331462));
#9062=CARTESIAN_POINT('Ctrl Pts',(8.63526635578534,-31.2053241874716,1.27285666375511));
#9063=CARTESIAN_POINT('Ctrl Pts',(9.11552542363584,-31.1754823150201,1.88762237576914));
#9064=CARTESIAN_POINT('Ctrl Pts',(9.59578449148634,-31.1456404425685,2.50238808778318));
#9065=CARTESIAN_POINT('Ctrl Pts',(10.2700943231832,-31.0037633093738,2.86933947451654));
#9066=CARTESIAN_POINT('Ctrl Pts',(10.9444041548801,-30.8618861761791,3.2362908612499));
#9067=CARTESIAN_POINT('Ctrl Pts',(11.7004303752665,-30.6728300639773,3.28274870019663));
#9068=CARTESIAN_POINT('Ctrl Pts',(12.4564565956529,-30.4837739517755,3.32920653914337));
#9069=CARTESIAN_POINT('Ctrl Pts',(13.1656798966061,-30.3217395177073,3.04596928553206));
#9070=CARTESIAN_POINT('Ctrl Pts',(13.8749031975594,-30.1597050836391,2.76273203192075));
#9071=CARTESIAN_POINT('Ctrl Pts',(14.4180741631509,-30.0935410100915,2.20589829750609));
#9072=CARTESIAN_POINT('Ctrl Pts',(14.9612451287424,-30.027376936544,1.64906456309142));
#9073=CARTESIAN_POINT('Ctrl Pts',(15.25200304456,-30.1069436052304,0.928922098091803));
#9074=CARTESIAN_POINT('Ctrl Pts',(15.5427609603776,-30.1865102739168,0.20877963309219));
#9075=CARTESIAN_POINT('Ctrl Pts',(15.5447386121598,-30.4328043057806,-0.532038515331461));
#9076=CARTESIAN_POINT('Ctrl Pts',(15.5467162639421,-30.6790983376445,-1.27285666375511));
#9077=CARTESIAN_POINT('Ctrl Pts',(15.2807429103773,-31.0800939545751,-1.88762237576914));
#9078=CARTESIAN_POINT('Ctrl Pts',(15.0147695568125,-31.4810895715057,-2.50238808778318));
#9079=CARTESIAN_POINT('Ctrl Pts',(14.5547454394014,-31.9941204491794,-2.86933947451654));
#9080=CARTESIAN_POINT('Ctrl Pts',(14.0947213219902,-32.5071513268532,-3.2362908612499));
#9081=CARTESIAN_POINT('Ctrl Pts',(13.5529808158895,-33.067361183534,-3.28274870019663));
#9082=CARTESIAN_POINT('Ctrl Pts',(13.0112403097889,-33.6275710402148,-3.32920653914337));
#9083=CARTESIAN_POINT('Ctrl Pts',(12.5163027231213,-34.1607592187621,-3.04596928553206));
#9084=CARTESIAN_POINT('Ctrl Pts',(12.0213651364537,-34.6939473973094,-2.76273203192075));
#9085=CARTESIAN_POINT('Ctrl Pts',(11.692479885148,-35.131265215336,-2.20589829750609));
#9086=CARTESIAN_POINT('Ctrl Pts',(11.3635946338422,-35.5685830333625,-1.64906456309142));
#9087=CARTESIAN_POINT('Ctrl Pts',(11.2871224323103,-35.8601701091552,-0.928922098091803));
#9088=CARTESIAN_POINT('Ctrl Pts',(11.2106502307784,-36.1517571849478,-0.208779633092189));
#9089=CARTESIAN_POINT('Ctrl Pts',(11.4229582932819,-36.2766168975631,0.532038515331462));
#9090=CARTESIAN_POINT('Ctrl Pts',(11.6352663557853,-36.4014766101783,1.27285666375511));
#9091=CARTESIAN_POINT('Ctrl Pts',(12.1155254236358,-36.3716347377267,1.88762237576914));
#9092=CARTESIAN_POINT('Ctrl Pts',(12.5957844914863,-36.3417928652752,2.50238808778318));
#9093=CARTESIAN_POINT('Ctrl Pts',(13.2700943231832,-36.1999157320805,2.86933947451654));
#9094=CARTESIAN_POINT('Ctrl Pts',(13.9444041548801,-36.0580385988858,3.2362908612499));
#9095=CARTESIAN_POINT('Ctrl Pts',(14.7004303752664,-35.868982486684,3.28274870019663));
#9096=CARTESIAN_POINT('Ctrl Pts',(15.4564565956528,-35.6799263744822,3.32920653914337));
#9097=CARTESIAN_POINT('Ctrl Pts',(16.1656798966061,-35.517891940414,3.04596928553206));
#9098=CARTESIAN_POINT('Ctrl Pts',(16.8749031975594,-35.3558575063457,2.76273203192075));
#9099=CARTESIAN_POINT('Ctrl Pts',(17.4180741631509,-35.2896934327982,2.20589829750609));
#9100=CARTESIAN_POINT('Ctrl Pts',(17.9612451287423,-35.2235293592507,1.64906456309142));
#9101=CARTESIAN_POINT('Ctrl Pts',(18.2520030445599,-35.3030960279371,0.928922098091803));
#9102=CARTESIAN_POINT('Ctrl Pts',(18.5427609603775,-35.3826626966235,0.20877963309219));
#9103=CARTESIAN_POINT('Ctrl Pts',(18.5447386121598,-35.6289567284873,-0.532038515331461));
#9104=CARTESIAN_POINT('Ctrl Pts',(18.5467162639421,-35.8752507603511,-1.27285666375511));
#9105=CARTESIAN_POINT('Ctrl Pts',(18.2807429103773,-36.2762463772817,-1.88762237576914));
#9106=CARTESIAN_POINT('Ctrl Pts',(18.0147695568125,-36.6772419942123,-2.50238808778318));
#9107=CARTESIAN_POINT('Ctrl Pts',(17.5547454394013,-37.1902728718861,-2.86933947451654));
#9108=CARTESIAN_POINT('Ctrl Pts',(17.0947213219902,-37.7033037495598,-3.2362908612499));
#9109=CARTESIAN_POINT('Ctrl Pts',(16.5529808158895,-38.2635136062407,-3.28274870019663));
#9110=CARTESIAN_POINT('Ctrl Pts',(16.0112403097889,-38.8237234629215,-3.32920653914337));
#9111=CARTESIAN_POINT('Ctrl Pts',(15.5163027231213,-39.3569116414688,-3.04596928553206));
#9112=CARTESIAN_POINT('Ctrl Pts',(15.0213651364537,-39.890099820016,-2.76273203192075));
#9113=CARTESIAN_POINT('Ctrl Pts',(14.6924798851479,-40.3274176380426,-2.20589829750609));
#9114=CARTESIAN_POINT('Ctrl Pts',(14.3635946338422,-40.7647354560692,-1.64906456309142));
#9115=CARTESIAN_POINT('Ctrl Pts',(14.2871224323103,-41.0563225318618,-0.928922098091803));
#9116=CARTESIAN_POINT('Ctrl Pts',(14.2106502307784,-41.3479096076545,-0.208779633092189));
#9117=CARTESIAN_POINT('Ctrl Pts',(14.4229582932818,-41.4727693202697,0.532038515331462));
#9118=CARTESIAN_POINT('Ctrl Pts',(14.6352663557853,-41.5976290328849,1.27285666375511));
#9119=CARTESIAN_POINT('Ctrl Pts',(15.1155254236358,-41.5677871604334,1.88762237576914));
#9120=CARTESIAN_POINT('Ctrl Pts',(15.5957844914863,-41.5379452879818,2.50238808778318));
#9121=CARTESIAN_POINT('Ctrl Pts',(16.2700943231832,-41.3960681547871,2.86933947451654));
#9122=CARTESIAN_POINT('Ctrl Pts',(16.94440415488,-41.2541910215924,3.2362908612499));
#9123=CARTESIAN_POINT('Ctrl Pts',(17.7004303752664,-41.0651349093906,3.28274870019663));
#9124=CARTESIAN_POINT('Ctrl Pts',(18.4564565956528,-40.8760787971888,3.32920653914337));
#9125=CARTESIAN_POINT('Ctrl Pts',(19.1656798966061,-40.7140443631206,3.04596928553206));
#9126=CARTESIAN_POINT('Ctrl Pts',(19.8749031975594,-40.5520099290524,2.76273203192075));
#9127=CARTESIAN_POINT('Ctrl Pts',(20.4180741631508,-40.4858458555049,2.20589829750609));
#9128=CARTESIAN_POINT('Ctrl Pts',(20.9612451287423,-40.4196817819573,1.64906456309142));
#9129=CARTESIAN_POINT('Ctrl Pts',(21.2520030445599,-40.4992484506437,0.928922098091803));
#9130=CARTESIAN_POINT('Ctrl Pts',(21.5427609603775,-40.5788151193301,0.20877963309219));
#9131=CARTESIAN_POINT('Ctrl Pts',(21.5447386121598,-40.8251091511939,-0.532038515331461));
#9132=CARTESIAN_POINT('Ctrl Pts',(21.546716263942,-41.0714031830578,-1.27285666375511));
#9133=CARTESIAN_POINT('Ctrl Pts',(21.2807429103773,-41.4723987999884,-1.88762237576914));
#9134=CARTESIAN_POINT('Ctrl Pts',(21.0147695568125,-41.873394416919,-2.50238808778318));
#9135=CARTESIAN_POINT('Ctrl Pts',(20.5547454394013,-42.3864252945927,-2.86933947451654));
#9136=CARTESIAN_POINT('Ctrl Pts',(20.0947213219901,-42.8994561722665,-3.2362908612499));
#9137=CARTESIAN_POINT('Ctrl Pts',(19.5529808158895,-43.4596660289473,-3.28274870019663));
#9138=CARTESIAN_POINT('Ctrl Pts',(19.0112403097888,-44.0198758856281,-3.32920653914337));
#9139=CARTESIAN_POINT('Ctrl Pts',(18.5163027231212,-44.5530640641754,-3.04596928553206));
#9140=CARTESIAN_POINT('Ctrl Pts',(18.0213651364537,-45.0862522427227,-2.76273203192075));
#9141=CARTESIAN_POINT('Ctrl Pts',(17.6924798851479,-45.5235700607493,-2.20589829750609));
#9142=CARTESIAN_POINT('Ctrl Pts',(3.62216201968442,-19.8058202438613,-1.94799199564959));
#9143=CARTESIAN_POINT('Ctrl Pts',(3.34425572651223,-20.2137053466864,-1.54490813204841));
#9144=CARTESIAN_POINT('Ctrl Pts',(3.25594179788809,-20.5121292468035,-0.988830267143717));
#9145=CARTESIAN_POINT('Ctrl Pts',(3.16762786926396,-20.8105531469205,-0.432752402239027));
#9146=CARTESIAN_POINT('Ctrl Pts',(3.3076189187292,-20.9771651064803,0.166181422977342));
#9147=CARTESIAN_POINT('Ctrl Pts',(3.44760996819445,-21.1437770660401,0.765115248193711));
#9148=CARTESIAN_POINT('Ctrl Pts',(3.80940000840298,-21.1823333185883,1.28827884419634));
#9149=CARTESIAN_POINT('Ctrl Pts',(4.17119004861151,-21.2208895711365,1.81144244019896));
#9150=CARTESIAN_POINT('Ctrl Pts',(4.70434308191443,-21.1605093534924,2.15521684061908));
#9151=CARTESIAN_POINT('Ctrl Pts',(5.23749611521735,-21.1001291358485,2.49899124103919));
#9152=CARTESIAN_POINT('Ctrl Pts',(5.8576356015542,-20.9895272661294,2.59528770975726));
#9153=CARTESIAN_POINT('Ctrl Pts',(6.47777508789106,-20.8789253964104,2.69158417847533));
#9154=CARTESIAN_POINT('Ctrl Pts',(7.08329575335921,-20.7767637068552,2.52133001886304));
#9155=CARTESIAN_POINT('Ctrl Pts',(7.68881641882736,-20.6746020173,2.35107585925076));
#9156=CARTESIAN_POINT('Ctrl Pts',(8.18100842628526,-20.6378706589539,1.94799199564959));
#9157=CARTESIAN_POINT('Ctrl Pts',(8.67320043374317,-20.6011393006078,1.54490813204841));
#9158=CARTESIAN_POINT('Ctrl Pts',(8.97580007665302,-20.6738691449698,0.988830267143717));
#9159=CARTESIAN_POINT('Ctrl Pts',(9.27839971956287,-20.7465989893318,0.432752402239027));
#9160=CARTESIAN_POINT('Ctrl Pts',(9.35269438438334,-20.9511407742511,-0.166181422977342));
#9161=CARTESIAN_POINT('Ctrl Pts',(9.4269890492038,-21.1556825591703,-0.765115248193711));
#9162=CARTESIAN_POINT('Ctrl Pts',(9.27948472328098,-21.4882800511012,-1.28827884419634));
#9163=CARTESIAN_POINT('Ctrl Pts',(9.13198039735816,-21.8208775430321,-1.81144244019896));
#9164=CARTESIAN_POINT('Ctrl Pts',(8.81311307834095,-22.2524115051551,-2.15521684061908));
#9165=CARTESIAN_POINT('Ctrl Pts',(8.49424575932375,-22.6839454672782,-2.49899124103919));
#9166=CARTESIAN_POINT('Ctrl Pts',(8.0883919872726,-23.1657010814762,-2.59528770975726));
#9167=CARTESIAN_POINT('Ctrl Pts',(7.68253821522146,-23.6474566956743,-2.69158417847533));
#9168=CARTESIAN_POINT('Ctrl Pts',(7.29130326403902,-24.1207721297085,-2.52133001886305));
#9169=CARTESIAN_POINT('Ctrl Pts',(6.90006831285659,-24.5940875637428,-2.35107585925076));
#9170=CARTESIAN_POINT('Ctrl Pts',(6.62216201968439,-25.0019726665679,-1.94799199564959));
#9171=CARTESIAN_POINT('Ctrl Pts',(6.34425572651219,-25.4098577693931,-1.54490813204841));
#9172=CARTESIAN_POINT('Ctrl Pts',(6.25594179788806,-25.7082816695101,-0.988830267143717));
#9173=CARTESIAN_POINT('Ctrl Pts',(6.16762786926392,-26.0067055696272,-0.432752402239027));
#9174=CARTESIAN_POINT('Ctrl Pts',(6.30761891872917,-26.1733175291869,0.166181422977342));
#9175=CARTESIAN_POINT('Ctrl Pts',(6.44760996819441,-26.3399294887468,0.765115248193711));
#9176=CARTESIAN_POINT('Ctrl Pts',(6.80940000840295,-26.3784857412949,1.28827884419634));
#9177=CARTESIAN_POINT('Ctrl Pts',(7.17119004861148,-26.4170419938431,1.81144244019896));
#9178=CARTESIAN_POINT('Ctrl Pts',(7.7043430819144,-26.3566617761991,2.15521684061908));
#9179=CARTESIAN_POINT('Ctrl Pts',(8.23749611521731,-26.2962815585551,2.49899124103919));
#9180=CARTESIAN_POINT('Ctrl Pts',(8.85763560155417,-26.1856796888361,2.59528770975726));
#9181=CARTESIAN_POINT('Ctrl Pts',(9.47777508789103,-26.0750778191171,2.69158417847533));
#9182=CARTESIAN_POINT('Ctrl Pts',(10.0832957533592,-25.9729161295619,2.52133001886304));
#9183=CARTESIAN_POINT('Ctrl Pts',(10.6888164188273,-25.8707544400067,2.35107585925076));
#9184=CARTESIAN_POINT('Ctrl Pts',(11.1810084262852,-25.8340230816606,1.94799199564959));
#9185=CARTESIAN_POINT('Ctrl Pts',(11.6732004337431,-25.7972917233145,1.54490813204841));
#9186=CARTESIAN_POINT('Ctrl Pts',(11.975800076653,-25.8700215676765,0.988830267143717));
#9187=CARTESIAN_POINT('Ctrl Pts',(12.2783997195628,-25.9427514120385,0.432752402239027));
#9188=CARTESIAN_POINT('Ctrl Pts',(12.3526943843833,-26.1472931969577,-0.166181422977342));
#9189=CARTESIAN_POINT('Ctrl Pts',(12.4269890492038,-26.351834981877,-0.765115248193711));
#9190=CARTESIAN_POINT('Ctrl Pts',(12.279484723281,-26.6844324738078,-1.28827884419634));
#9191=CARTESIAN_POINT('Ctrl Pts',(12.1319803973581,-27.0170299657387,-1.81144244019896));
#9192=CARTESIAN_POINT('Ctrl Pts',(11.8131130783409,-27.4485639278618,-2.15521684061908));
#9193=CARTESIAN_POINT('Ctrl Pts',(11.4942457593237,-27.8800978899848,-2.49899124103919));
#9194=CARTESIAN_POINT('Ctrl Pts',(11.0883919872726,-28.3618535041829,-2.59528770975726));
#9195=CARTESIAN_POINT('Ctrl Pts',(10.6825382152214,-28.8436091183809,-2.69158417847533));
#9196=CARTESIAN_POINT('Ctrl Pts',(10.291303264039,-29.3169245524152,-2.52133001886305));
#9197=CARTESIAN_POINT('Ctrl Pts',(9.90006831285655,-29.7902399864494,-2.35107585925076));
#9198=CARTESIAN_POINT('Ctrl Pts',(9.62216201968436,-30.1981250892746,-1.94799199564959));
#9199=CARTESIAN_POINT('Ctrl Pts',(9.34425572651217,-30.6060101920997,-1.54490813204841));
#9200=CARTESIAN_POINT('Ctrl Pts',(9.25594179788803,-30.9044340922168,-0.988830267143717));
#9201=CARTESIAN_POINT('Ctrl Pts',(9.16762786926389,-31.2028579923338,-0.432752402239027));
#9202=CARTESIAN_POINT('Ctrl Pts',(9.30761891872914,-31.3694699518936,0.166181422977342));
#9203=CARTESIAN_POINT('Ctrl Pts',(9.44760996819438,-31.5360819114534,0.765115248193711));
#9204=CARTESIAN_POINT('Ctrl Pts',(9.80940000840292,-31.5746381640016,1.28827884419634));
#9205=CARTESIAN_POINT('Ctrl Pts',(10.1711900486115,-31.6131944165497,1.81144244019896));
#9206=CARTESIAN_POINT('Ctrl Pts',(10.7043430819144,-31.5528141989058,2.15521684061908));
#9207=CARTESIAN_POINT('Ctrl Pts',(11.2374961152173,-31.4924339812617,2.49899124103919));
#9208=CARTESIAN_POINT('Ctrl Pts',(11.8576356015541,-31.3818321115427,2.59528770975726));
#9209=CARTESIAN_POINT('Ctrl Pts',(12.477775087891,-31.2712302418237,2.69158417847533));
#9210=CARTESIAN_POINT('Ctrl Pts',(13.0832957533591,-31.1690685522685,2.52133001886304));
#9211=CARTESIAN_POINT('Ctrl Pts',(13.6888164188273,-31.0669068627133,2.35107585925076));
#9212=CARTESIAN_POINT('Ctrl Pts',(14.1810084262852,-31.0301755043672,1.94799199564959));
#9213=CARTESIAN_POINT('Ctrl Pts',(14.6732004337431,-30.9934441460211,1.54490813204841));
#9214=CARTESIAN_POINT('Ctrl Pts',(14.975800076653,-31.0661739903831,0.988830267143717));
#9215=CARTESIAN_POINT('Ctrl Pts',(15.2783997195628,-31.1389038347451,0.432752402239027));
#9216=CARTESIAN_POINT('Ctrl Pts',(15.3526943843833,-31.3434456196644,-0.166181422977342));
#9217=CARTESIAN_POINT('Ctrl Pts',(15.4269890492037,-31.5479874045836,-0.765115248193711));
#9218=CARTESIAN_POINT('Ctrl Pts',(15.2794847232809,-31.8805848965145,-1.28827884419634));
#9219=CARTESIAN_POINT('Ctrl Pts',(15.1319803973581,-32.2131823884454,-1.81144244019896));
#9220=CARTESIAN_POINT('Ctrl Pts',(14.8131130783409,-32.6447163505684,-2.15521684061908));
#9221=CARTESIAN_POINT('Ctrl Pts',(14.4942457593237,-33.0762503126915,-2.49899124103919));
#9222=CARTESIAN_POINT('Ctrl Pts',(14.0883919872725,-33.5580059268895,-2.59528770975726));
#9223=CARTESIAN_POINT('Ctrl Pts',(13.6825382152214,-34.0397615410876,-2.69158417847533));
#9224=CARTESIAN_POINT('Ctrl Pts',(13.291303264039,-34.5130769751218,-2.52133001886305));
#9225=CARTESIAN_POINT('Ctrl Pts',(12.9000683128565,-34.9863924091561,-2.35107585925076));
#9226=CARTESIAN_POINT('Ctrl Pts',(12.6221620196843,-35.3942775119812,-1.94799199564959));
#9227=CARTESIAN_POINT('Ctrl Pts',(12.3442557265121,-35.8021626148064,-1.54490813204841));
#9228=CARTESIAN_POINT('Ctrl Pts',(12.255941797888,-36.1005865149234,-0.988830267143717));
#9229=CARTESIAN_POINT('Ctrl Pts',(12.1676278692639,-36.3990104150405,-0.432752402239027));
#9230=CARTESIAN_POINT('Ctrl Pts',(12.3076189187291,-36.5656223746002,0.166181422977342));
#9231=CARTESIAN_POINT('Ctrl Pts',(12.4476099681944,-36.73223433416,0.765115248193711));
#9232=CARTESIAN_POINT('Ctrl Pts',(12.8094000084029,-36.7707905867082,1.28827884419634));
#9233=CARTESIAN_POINT('Ctrl Pts',(13.1711900486114,-36.8093468392564,1.81144244019896));
#9234=CARTESIAN_POINT('Ctrl Pts',(13.7043430819143,-36.7489666216124,2.15521684061908));
#9235=CARTESIAN_POINT('Ctrl Pts',(14.2374961152173,-36.6885864039684,2.49899124103919));
#9236=CARTESIAN_POINT('Ctrl Pts',(14.8576356015541,-36.5779845342494,2.59528770975726));
#9237=CARTESIAN_POINT('Ctrl Pts',(15.477775087891,-36.4673826645304,2.69158417847533));
#9238=CARTESIAN_POINT('Ctrl Pts',(16.0832957533591,-36.3652209749752,2.52133001886304));
#9239=CARTESIAN_POINT('Ctrl Pts',(16.6888164188273,-36.26305928542,2.35107585925076));
#9240=CARTESIAN_POINT('Ctrl Pts',(17.1810084262852,-36.2263279270739,1.94799199564959));
#9241=CARTESIAN_POINT('Ctrl Pts',(17.6732004337431,-36.1895965687278,1.54490813204841));
#9242=CARTESIAN_POINT('Ctrl Pts',(17.9758000766529,-36.2623264130898,0.988830267143717));
#9243=CARTESIAN_POINT('Ctrl Pts',(18.2783997195628,-36.3350562574518,0.432752402239027));
#9244=CARTESIAN_POINT('Ctrl Pts',(18.3526943843832,-36.539598042371,-0.166181422977342));
#9245=CARTESIAN_POINT('Ctrl Pts',(18.4269890492037,-36.7441398272903,-0.765115248193711));
#9246=CARTESIAN_POINT('Ctrl Pts',(18.2794847232809,-37.0767373192211,-1.28827884419634));
#9247=CARTESIAN_POINT('Ctrl Pts',(18.1319803973581,-37.409334811152,-1.81144244019896));
#9248=CARTESIAN_POINT('Ctrl Pts',(17.8131130783409,-37.8408687732751,-2.15521684061908));
#9249=CARTESIAN_POINT('Ctrl Pts',(17.4942457593237,-38.2724027353981,-2.49899124103919));
#9250=CARTESIAN_POINT('Ctrl Pts',(17.0883919872725,-38.7541583495962,-2.59528770975726));
#9251=CARTESIAN_POINT('Ctrl Pts',(16.6825382152214,-39.2359139637942,-2.69158417847533));
#9252=CARTESIAN_POINT('Ctrl Pts',(16.2913032640389,-39.7092293978285,-2.52133001886305));
#9253=CARTESIAN_POINT('Ctrl Pts',(15.9000683128565,-40.1825448318627,-2.35107585925076));
#9254=CARTESIAN_POINT('Ctrl Pts',(15.6221620196843,-40.5904299346879,-1.94799199564959));
#9255=CARTESIAN_POINT('Ctrl Pts',(15.3442557265121,-40.998315037513,-1.54490813204841));
#9256=CARTESIAN_POINT('Ctrl Pts',(15.255941797888,-41.2967389376301,-0.988830267143717));
#9257=CARTESIAN_POINT('Ctrl Pts',(15.1676278692638,-41.5951628377471,-0.432752402239027));
#9258=CARTESIAN_POINT('Ctrl Pts',(15.3076189187291,-41.7617747973069,0.166181422977342));
#9259=CARTESIAN_POINT('Ctrl Pts',(15.4476099681943,-41.9283867568667,0.765115248193711));
#9260=CARTESIAN_POINT('Ctrl Pts',(15.8094000084029,-41.9669430094149,1.28827884419634));
#9261=CARTESIAN_POINT('Ctrl Pts',(16.1711900486114,-42.0054992619631,1.81144244019896));
#9262=CARTESIAN_POINT('Ctrl Pts',(16.7043430819143,-41.945119044319,2.15521684061908));
#9263=CARTESIAN_POINT('Ctrl Pts',(17.2374961152172,-41.884738826675,2.49899124103919));
#9264=CARTESIAN_POINT('Ctrl Pts',(17.8576356015541,-41.774136956956,2.59528770975726));
#9265=CARTESIAN_POINT('Ctrl Pts',(18.4777750878909,-41.6635350872371,2.69158417847533));
#9266=CARTESIAN_POINT('Ctrl Pts',(19.0832957533591,-41.5613733976818,2.52133001886304));
#9267=CARTESIAN_POINT('Ctrl Pts',(19.6888164188272,-41.4592117081266,2.35107585925076));
#9268=CARTESIAN_POINT('Ctrl Pts',(20.1810084262851,-41.4224803497805,1.94799199564959));
#9269=CARTESIAN_POINT('Ctrl Pts',(20.673200433743,-41.3857489914344,1.54490813204841));
#9270=CARTESIAN_POINT('Ctrl Pts',(20.9758000766529,-41.4584788357964,0.988830267143717));
#9271=CARTESIAN_POINT('Ctrl Pts',(21.2783997195627,-41.5312086801584,0.432752402239027));
#9272=CARTESIAN_POINT('Ctrl Pts',(21.3526943843832,-41.7357504650777,-0.166181422977342));
#9273=CARTESIAN_POINT('Ctrl Pts',(21.4269890492037,-41.940292249997,-0.765115248193711));
#9274=CARTESIAN_POINT('Ctrl Pts',(21.2794847232809,-42.2728897419278,-1.28827884419634));
#9275=CARTESIAN_POINT('Ctrl Pts',(21.131980397358,-42.6054872338587,-1.81144244019896));
#9276=CARTESIAN_POINT('Ctrl Pts',(20.8131130783408,-43.0370211959817,-2.15521684061908));
#9277=CARTESIAN_POINT('Ctrl Pts',(20.4942457593236,-43.4685551581048,-2.49899124103919));
#9278=CARTESIAN_POINT('Ctrl Pts',(20.0883919872725,-43.9503107723028,-2.59528770975726));
#9279=CARTESIAN_POINT('Ctrl Pts',(19.6825382152213,-44.4320663865008,-2.69158417847533));
#9280=CARTESIAN_POINT('Ctrl Pts',(19.2913032640389,-44.9053818205351,-2.52133001886305));
#9281=CARTESIAN_POINT('Ctrl Pts',(18.9000683128565,-45.3786972545694,-2.35107585925076));
#9282=CARTESIAN_POINT('Ctrl Pts',(18.6221620196843,-45.7865823573945,-1.94799199564959));
#9283=CARTESIAN_POINT('',(0.,0.,0.));
#9284=CARTESIAN_POINT('Origin',(0.,0.,-4.5));
#9285=CARTESIAN_POINT('',(-1.25,-1.53080849893419E-16,-0.5));
#9286=CARTESIAN_POINT('Origin',(0.,0.,-0.5));
#9287=CARTESIAN_POINT('',(-1.25,-1.53080849893419E-16,0.5));
#9288=CARTESIAN_POINT('',(-1.25,-1.53080849893419E-16,-4.5));
#9289=CARTESIAN_POINT('Origin',(0.,0.,0.5));
#9290=CARTESIAN_POINT('Origin',(0.,-2.,0.5));
#9291=CARTESIAN_POINT('',(-17.1201286922563,-2.,-0.5));
#9292=CARTESIAN_POINT('',(-17.1201286922563,-2.,0.5));
#9293=CARTESIAN_POINT('',(-17.1201286922563,-2.,-0.5));
#9294=CARTESIAN_POINT('',(-17.6201286922563,-2.,0.5));
#9295=CARTESIAN_POINT('',(2.44929359829471E-16,-2.,0.5));
#9296=CARTESIAN_POINT('',(-17.6201286922563,-2.,-0.5));
#9297=CARTESIAN_POINT('',(-17.6201286922563,-2.,-0.5));
#9298=CARTESIAN_POINT('',(0.,-2.,-0.5));
#9299=CARTESIAN_POINT('Origin',(0.,-2.,0.5));
#9300=CARTESIAN_POINT('',(-16.6201286922563,-2.,-0.5));
#9301=CARTESIAN_POINT('',(-16.6201286922563,-2.,0.5));
#9302=CARTESIAN_POINT('',(-16.6201286922563,-2.,-0.5));
#9303=CARTESIAN_POINT('',(-16.1201286922563,-2.,-0.5));
#9304=CARTESIAN_POINT('',(0.,-2.,-0.5));
#9305=CARTESIAN_POINT('',(-16.1201286922563,-2.,0.5));
#9306=CARTESIAN_POINT('',(-16.1201286922563,-2.,-0.5));
#9307=CARTESIAN_POINT('',(2.44929359829471E-16,-2.,0.5));
#9308=CARTESIAN_POINT('Origin',(0.,-2.,0.5));
#9309=CARTESIAN_POINT('',(-15.6201286922563,-2.,-0.5));
#9310=CARTESIAN_POINT('',(-15.6201286922563,-2.,0.5));
#9311=CARTESIAN_POINT('',(-15.6201286922563,-2.,-0.5));
#9312=CARTESIAN_POINT('',(-15.1201286922563,-2.,-0.5));
#9313=CARTESIAN_POINT('',(0.,-2.,-0.5));
#9314=CARTESIAN_POINT('',(-15.1201286922563,-2.,0.5));
#9315=CARTESIAN_POINT('',(-15.1201286922563,-2.,-0.5));
#9316=CARTESIAN_POINT('',(2.44929359829471E-16,-2.,0.5));
#9317=CARTESIAN_POINT('Origin',(0.,-2.,0.5));
#9318=CARTESIAN_POINT('',(-14.6201286922563,-2.,-0.5));
#9319=CARTESIAN_POINT('',(-14.6201286922563,-2.,0.5));
#9320=CARTESIAN_POINT('',(-14.6201286922563,-2.,-0.5));
#9321=CARTESIAN_POINT('',(-14.1201286922563,-2.,-0.5));
#9322=CARTESIAN_POINT('',(0.,-2.,-0.5));
#9323=CARTESIAN_POINT('',(-14.1201286922563,-2.,0.5));
#9324=CARTESIAN_POINT('',(-14.1201286922563,-2.,-0.5));
#9325=CARTESIAN_POINT('',(2.44929359829471E-16,-2.,0.5));
#9326=CARTESIAN_POINT('Origin',(0.,-2.,0.5));
#9327=CARTESIAN_POINT('',(-13.6201286922563,-2.,-0.5));
#9328=CARTESIAN_POINT('',(-13.6201286922563,-2.,0.5));
#9329=CARTESIAN_POINT('',(-13.6201286922563,-2.,-0.5));
#9330=CARTESIAN_POINT('',(-13.1201286922563,-2.,-0.5));
#9331=CARTESIAN_POINT('',(0.,-2.,-0.5));
#9332=CARTESIAN_POINT('',(-13.1201286922563,-2.,0.5));
#9333=CARTESIAN_POINT('',(-13.1201286922563,-2.,-0.5));
#9334=CARTESIAN_POINT('',(2.44929359829471E-16,-2.,0.5));
#9335=CARTESIAN_POINT('Origin',(0.,-2.,0.5));
#9336=CARTESIAN_POINT('',(-12.6201286922563,-2.,-0.5));
#9337=CARTESIAN_POINT('',(-12.6201286922563,-2.,0.5));
#9338=CARTESIAN_POINT('',(-12.6201286922563,-2.,-0.5));
#9339=CARTESIAN_POINT('',(-12.1201286922563,-2.,-0.5));
#9340=CARTESIAN_POINT('',(0.,-2.,-0.5));
#9341=CARTESIAN_POINT('',(-12.1201286922563,-2.,0.5));
#9342=CARTESIAN_POINT('',(-12.1201286922563,-2.,-0.5));
#9343=CARTESIAN_POINT('',(2.44929359829471E-16,-2.,0.5));
#9344=CARTESIAN_POINT('Origin',(0.,-2.,0.5));
#9345=CARTESIAN_POINT('',(-11.6201286922563,-2.,-0.5));
#9346=CARTESIAN_POINT('',(-11.6201286922563,-2.,0.5));
#9347=CARTESIAN_POINT('',(-11.6201286922563,-2.,-0.5));
#9348=CARTESIAN_POINT('',(-11.1201286922563,-2.,-0.5));
#9349=CARTESIAN_POINT('',(0.,-2.,-0.5));
#9350=CARTESIAN_POINT('',(-11.1201286922563,-2.,0.5));
#9351=CARTESIAN_POINT('',(-11.1201286922563,-2.,-0.5));
#9352=CARTESIAN_POINT('',(2.44929359829471E-16,-2.,0.5));
#9353=CARTESIAN_POINT('Origin',(0.,-2.,0.5));
#9354=CARTESIAN_POINT('',(-10.6201286922563,-2.,-0.5));
#9355=CARTESIAN_POINT('',(-10.6201286922563,-2.,0.5));
#9356=CARTESIAN_POINT('',(-10.6201286922563,-2.,-0.5));
#9357=CARTESIAN_POINT('',(-10.1201286922563,-2.,-0.5));
#9358=CARTESIAN_POINT('',(0.,-2.,-0.5));
#9359=CARTESIAN_POINT('',(-10.1201286922563,-2.,0.5));
#9360=CARTESIAN_POINT('',(-10.1201286922563,-2.,-0.5));
#9361=CARTESIAN_POINT('',(2.44929359829471E-16,-2.,0.5));
#9362=CARTESIAN_POINT('Origin',(0.,-2.,0.5));
#9363=CARTESIAN_POINT('',(-9.6201286922563,-2.,-0.5));
#9364=CARTESIAN_POINT('',(-9.6201286922563,-2.,0.5));
#9365=CARTESIAN_POINT('',(-9.6201286922563,-2.,-0.5));
#9366=CARTESIAN_POINT('',(-9.1201286922563,-2.,-0.5));
#9367=CARTESIAN_POINT('',(0.,-2.,-0.5));
#9368=CARTESIAN_POINT('',(-9.1201286922563,-2.,0.5));
#9369=CARTESIAN_POINT('',(-9.1201286922563,-2.,-0.5));
#9370=CARTESIAN_POINT('',(2.44929359829471E-16,-2.,0.5));
#9371=CARTESIAN_POINT('Origin',(0.,-2.,0.5));
#9372=CARTESIAN_POINT('',(-18.1201286922563,-2.,-0.5));
#9373=CARTESIAN_POINT('',(-18.3701286922563,-2.,-0.5));
#9374=CARTESIAN_POINT('',(0.,-2.,-0.5));
#9375=CARTESIAN_POINT('',(-18.1201286922563,-2.,0.5));
#9376=CARTESIAN_POINT('',(-18.1201286922563,-2.,-0.5));
#9377=CARTESIAN_POINT('',(-18.3701286922563,-2.,0.5));
#9378=CARTESIAN_POINT('',(2.44929359829471E-16,-2.,0.5));
#9379=CARTESIAN_POINT('',(-18.3701286922563,-2.,0.5));
#9380=CARTESIAN_POINT('Origin',(0.,-2.,0.5));
#9381=CARTESIAN_POINT('',(-8.6201286922563,-2.,-0.5));
#9382=CARTESIAN_POINT('',(-8.6201286922563,-2.,0.5));
#9383=CARTESIAN_POINT('',(-8.6201286922563,-2.,-0.5));
#9384=CARTESIAN_POINT('',(3.,-2.,-0.5));
#9385=CARTESIAN_POINT('',(0.,-2.,-0.5));
#9386=CARTESIAN_POINT('',(3.,-2.,0.5));
#9387=CARTESIAN_POINT('',(3.,-2.,0.5));
#9388=CARTESIAN_POINT('',(2.44929359829471E-16,-2.,0.5));
#9389=CARTESIAN_POINT('Origin',(3.,2.,0.5));
#9390=CARTESIAN_POINT('',(3.,2.,-0.5));
#9391=CARTESIAN_POINT('',(3.,2.,-0.5));
#9392=CARTESIAN_POINT('',(3.,2.,0.5));
#9393=CARTESIAN_POINT('',(3.,2.,0.5));
#9394=CARTESIAN_POINT('',(3.,2.,0.5));
#9395=CARTESIAN_POINT('Origin',(0.,2.,0.5));
#9396=CARTESIAN_POINT('',(-7.83447493940356,2.,-0.5));
#9397=CARTESIAN_POINT('',(0.,2.,-0.5));
#9398=CARTESIAN_POINT('',(-7.83447493940357,2.,0.5));
#9399=CARTESIAN_POINT('',(-7.83447493940356,2.,0.5));
#9400=CARTESIAN_POINT('',(-2.44929359829471E-16,2.,0.5));
#9401=CARTESIAN_POINT('Origin',(0.,0.,0.5));
#9402=CARTESIAN_POINT('',(0.,-2.,0.5));
#9403=CARTESIAN_POINT('',(1.,-2.,0.5));
#9404=CARTESIAN_POINT('',(2.,-2.,0.5));
#9405=CARTESIAN_POINT('',(3.,-2.,0.5));
#9406=CARTESIAN_POINT('',(4.,-2.,0.5));
#9407=CARTESIAN_POINT('',(5.,-2.,0.5));
#9408=CARTESIAN_POINT('',(6.,-2.,0.5));
#9409=CARTESIAN_POINT('',(7.,-2.,0.5));
#9410=CARTESIAN_POINT('',(8.,-2.,0.5));
#9411=CARTESIAN_POINT('',(9.,-2.,0.5));
#9412=CARTESIAN_POINT('',(-18.6335200360776,-1.075,0.5));
#9413=CARTESIAN_POINT('Origin',(-7.83447493940356,-18.5,0.5));
#9414=CARTESIAN_POINT('Origin',(-18.3701286922563,-1.5,0.5));
#9415=CARTESIAN_POINT('Origin',(0.,0.,-0.5));
#9416=CARTESIAN_POINT('',(-9.1201286922563,-2.,-0.5));
#9417=CARTESIAN_POINT('',(-10.1201286922563,-2.,-0.5));
#9418=CARTESIAN_POINT('',(-11.1201286922563,-2.,-0.5));
#9419=CARTESIAN_POINT('',(-12.1201286922563,-2.,-0.5));
#9420=CARTESIAN_POINT('',(-13.1201286922563,-2.,-0.5));
#9421=CARTESIAN_POINT('',(-14.1201286922563,-2.,-0.5));
#9422=CARTESIAN_POINT('',(-15.1201286922563,-2.,-0.5));
#9423=CARTESIAN_POINT('',(-16.1201286922563,-2.,-0.5));
#9424=CARTESIAN_POINT('',(-17.1201286922563,-2.,-0.5));
#9425=CARTESIAN_POINT('',(-18.1201286922563,-2.,-0.5));
#9426=CARTESIAN_POINT('',(-18.6335200360776,-1.075,-0.5));
#9427=CARTESIAN_POINT('Origin',(-18.3701286922563,-1.5,-0.5));
#9428=CARTESIAN_POINT('Origin',(-7.83447493940356,-18.5,-0.5));
#9429=CARTESIAN_POINT('Origin',(-7.83447493940356,-18.5,0.5));
#9430=CARTESIAN_POINT('',(-18.6335200360776,-1.075,0.5));
#9431=CARTESIAN_POINT('Origin',(-18.3701286922563,-1.5,0.5));
#9432=CARTESIAN_POINT('Origin',(-18.1201286922563,-2.,-0.5));
#9433=CARTESIAN_POINT('',(-18.1201286922563,-2.5,-4.33680868994202E-16));
#9434=CARTESIAN_POINT('',(-18.1201286922563,-2.,-0.5));
#9435=CARTESIAN_POINT('',(-18.1201286922563,-2.5,-2.16840434497101E-16));
#9436=CARTESIAN_POINT('Origin',(-17.6201286922563,-2.5,-4.33680868994202E-16));
#9437=CARTESIAN_POINT('',(-17.9534620255896,-2.33333333333333,0.166666666666666));
#9438=CARTESIAN_POINT('Origin',(-18.1201286922563,-2.5,-0.5));
#9439=CARTESIAN_POINT('',(-17.9534620255896,-2.33333333333333,-0.166666666666666));
#9440=CARTESIAN_POINT('Origin',(0.,-2.,-0.5));
#9441=CARTESIAN_POINT('Origin',(-9.1201286922563,-2.,-0.5));
#9442=CARTESIAN_POINT('',(-9.1201286922563,-2.5,-4.33680868994202E-16));
#9443=CARTESIAN_POINT('',(-9.1201286922563,-2.,-0.5));
#9444=CARTESIAN_POINT('',(-9.1201286922563,-2.5,-2.16840434497101E-16));
#9445=CARTESIAN_POINT('Origin',(-8.6201286922563,-2.5,-4.33680868994202E-16));
#9446=CARTESIAN_POINT('',(-8.95346202558963,-2.33333333333333,0.166666666666666));
#9447=CARTESIAN_POINT('Origin',(-9.1201286922563,-2.5,-0.5));
#9448=CARTESIAN_POINT('',(-8.95346202558963,-2.33333333333333,-0.166666666666666));
#9449=CARTESIAN_POINT('Origin',(9.,-2.,-0.5));
#9450=CARTESIAN_POINT('Origin',(-10.1201286922563,-2.,-0.5));
#9451=CARTESIAN_POINT('',(-10.1201286922563,-2.5,-4.33680868994202E-16));
#9452=CARTESIAN_POINT('',(-10.1201286922563,-2.,-0.5));
#9453=CARTESIAN_POINT('',(-10.1201286922563,-2.5,-2.16840434497101E-16));
#9454=CARTESIAN_POINT('Origin',(-9.6201286922563,-2.5,-4.33680868994202E-16));
#9455=CARTESIAN_POINT('',(-9.95346202558963,-2.33333333333333,0.166666666666666));
#9456=CARTESIAN_POINT('Origin',(-10.1201286922563,-2.5,-0.5));
#9457=CARTESIAN_POINT('',(-9.95346202558963,-2.33333333333333,-0.166666666666666));
#9458=CARTESIAN_POINT('Origin',(8.,-2.,-0.5));
#9459=CARTESIAN_POINT('Origin',(-11.1201286922563,-2.,-0.5));
#9460=CARTESIAN_POINT('',(-11.1201286922563,-2.5,-4.33680868994202E-16));
#9461=CARTESIAN_POINT('',(-11.1201286922563,-2.,-0.5));
#9462=CARTESIAN_POINT('',(-11.1201286922563,-2.5,-2.16840434497101E-16));
#9463=CARTESIAN_POINT('Origin',(-10.6201286922563,-2.5,-4.33680868994202E-16));
#9464=CARTESIAN_POINT('',(-10.9534620255896,-2.33333333333333,0.166666666666666));
#9465=CARTESIAN_POINT('Origin',(-11.1201286922563,-2.5,-0.5));
#9466=CARTESIAN_POINT('',(-10.9534620255896,-2.33333333333333,-0.166666666666666));
#9467=CARTESIAN_POINT('Origin',(7.,-2.,-0.5));
#9468=CARTESIAN_POINT('Origin',(-12.1201286922563,-2.,-0.5));
#9469=CARTESIAN_POINT('',(-12.1201286922563,-2.5,-4.33680868994202E-16));
#9470=CARTESIAN_POINT('',(-12.1201286922563,-2.,-0.5));
#9471=CARTESIAN_POINT('',(-12.1201286922563,-2.5,-2.16840434497101E-16));
#9472=CARTESIAN_POINT('Origin',(-11.6201286922563,-2.5,-4.33680868994202E-16));
#9473=CARTESIAN_POINT('',(-11.9534620255896,-2.33333333333333,0.166666666666666));
#9474=CARTESIAN_POINT('Origin',(-12.1201286922563,-2.5,-0.5));
#9475=CARTESIAN_POINT('',(-11.9534620255896,-2.33333333333333,-0.166666666666666));
#9476=CARTESIAN_POINT('Origin',(6.,-2.,-0.5));
#9477=CARTESIAN_POINT('Origin',(-13.1201286922563,-2.,-0.5));
#9478=CARTESIAN_POINT('',(-13.1201286922563,-2.5,-4.33680868994202E-16));
#9479=CARTESIAN_POINT('',(-13.1201286922563,-2.,-0.5));
#9480=CARTESIAN_POINT('',(-13.1201286922563,-2.5,-2.16840434497101E-16));
#9481=CARTESIAN_POINT('Origin',(-12.6201286922563,-2.5,-4.33680868994202E-16));
#9482=CARTESIAN_POINT('',(-12.9534620255896,-2.33333333333333,0.166666666666666));
#9483=CARTESIAN_POINT('Origin',(-13.1201286922563,-2.5,-0.5));
#9484=CARTESIAN_POINT('',(-12.9534620255896,-2.33333333333333,-0.166666666666666));
#9485=CARTESIAN_POINT('Origin',(5.,-2.,-0.5));
#9486=CARTESIAN_POINT('Origin',(-14.1201286922563,-2.,-0.5));
#9487=CARTESIAN_POINT('',(-14.1201286922563,-2.5,-4.33680868994202E-16));
#9488=CARTESIAN_POINT('',(-14.1201286922563,-2.,-0.5));
#9489=CARTESIAN_POINT('',(-14.1201286922563,-2.5,-2.16840434497101E-16));
#9490=CARTESIAN_POINT('Origin',(-13.6201286922563,-2.5,-4.33680868994202E-16));
#9491=CARTESIAN_POINT('',(-13.9534620255896,-2.33333333333333,0.166666666666666));
#9492=CARTESIAN_POINT('Origin',(-14.1201286922563,-2.5,-0.5));
#9493=CARTESIAN_POINT('',(-13.9534620255896,-2.33333333333333,-0.166666666666666));
#9494=CARTESIAN_POINT('Origin',(4.,-2.,-0.5));
#9495=CARTESIAN_POINT('Origin',(-15.1201286922563,-2.,-0.5));
#9496=CARTESIAN_POINT('',(-15.1201286922563,-2.5,-4.33680868994202E-16));
#9497=CARTESIAN_POINT('',(-15.1201286922563,-2.,-0.5));
#9498=CARTESIAN_POINT('',(-15.1201286922563,-2.5,-2.16840434497101E-16));
#9499=CARTESIAN_POINT('Origin',(-14.6201286922563,-2.5,-4.33680868994202E-16));
#9500=CARTESIAN_POINT('',(-14.9534620255896,-2.33333333333333,0.166666666666666));
#9501=CARTESIAN_POINT('Origin',(-15.1201286922563,-2.5,-0.5));
#9502=CARTESIAN_POINT('',(-14.9534620255896,-2.33333333333333,-0.166666666666666));
#9503=CARTESIAN_POINT('Origin',(3.,-2.,-0.5));
#9504=CARTESIAN_POINT('Origin',(-16.1201286922563,-2.,-0.5));
#9505=CARTESIAN_POINT('',(-16.1201286922563,-2.5,-4.33680868994202E-16));
#9506=CARTESIAN_POINT('',(-16.1201286922563,-2.,-0.5));
#9507=CARTESIAN_POINT('',(-16.1201286922563,-2.5,-2.16840434497101E-16));
#9508=CARTESIAN_POINT('Origin',(-15.6201286922563,-2.5,-4.33680868994202E-16));
#9509=CARTESIAN_POINT('',(-15.9534620255896,-2.33333333333333,0.166666666666666));
#9510=CARTESIAN_POINT('Origin',(-16.1201286922563,-2.5,-0.5));
#9511=CARTESIAN_POINT('',(-15.9534620255896,-2.33333333333333,-0.166666666666666));
#9512=CARTESIAN_POINT('Origin',(2.,-2.,-0.5));
#9513=CARTESIAN_POINT('Origin',(-17.1201286922563,-2.,-0.5));
#9514=CARTESIAN_POINT('',(-17.1201286922563,-2.5,-4.33680868994202E-16));
#9515=CARTESIAN_POINT('',(-17.1201286922563,-2.,-0.5));
#9516=CARTESIAN_POINT('',(-17.1201286922563,-2.5,-2.16840434497101E-16));
#9517=CARTESIAN_POINT('Origin',(-16.6201286922563,-2.5,-4.33680868994202E-16));
#9518=CARTESIAN_POINT('',(-16.9534620255896,-2.33333333333333,0.166666666666666));
#9519=CARTESIAN_POINT('Origin',(-17.1201286922563,-2.5,-0.5));
#9520=CARTESIAN_POINT('',(-16.9534620255896,-2.33333333333333,-0.166666666666666));
#9521=CARTESIAN_POINT('Origin',(1.,-2.,-0.5));
#9522=CARTESIAN_POINT('',(0.,0.,0.));
#9523=CARTESIAN_POINT('Origin',(0.,0.,4.5));
#9524=CARTESIAN_POINT('',(1.25,-1.53080849893419E-16,-4.5));
#9525=CARTESIAN_POINT('Origin',(0.,0.,-4.5));
#9526=CARTESIAN_POINT('',(1.25,-1.53080849893419E-16,4.5));
#9527=CARTESIAN_POINT('',(1.25,-1.53080849893419E-16,4.5));
#9528=CARTESIAN_POINT('Origin',(0.,0.,4.5));
#9529=CARTESIAN_POINT('Origin',(0.,0.,4.5));
#9530=CARTESIAN_POINT('Origin',(0.,0.,-4.5));
#9531=CARTESIAN_POINT('',(0.,0.,0.));
#9532=CARTESIAN_POINT('Origin',(0.,-10.,3.5));
#9533=CARTESIAN_POINT('',(1.5,-10.,-3.5));
#9534=CARTESIAN_POINT('Origin',(0.,-10.,-3.5));
#9535=CARTESIAN_POINT('',(1.5,-10.,3.5));
#9536=CARTESIAN_POINT('',(1.5,-10.,3.5));
#9537=CARTESIAN_POINT('Origin',(0.,-10.,3.5));
#9538=CARTESIAN_POINT('Origin',(0.,-10.,3.5));
#9539=CARTESIAN_POINT('Origin',(0.,-10.,-3.5));
#9540=CARTESIAN_POINT('',(0.,0.,0.));
#9541=CARTESIAN_POINT('',(0.,0.,0.));
#9542=CARTESIAN_POINT('',(0.,0.,0.));
#9543=CARTESIAN_POINT('',(0.,0.,0.));
#9544=CARTESIAN_POINT('',(0.,0.,0.));
#9545=CARTESIAN_POINT('',(0.,0.,0.));
#9546=UNCERTAINTY_MEASURE_WITH_UNIT(LENGTH_MEASURE(0.01),#9562,
'DISTANCE_ACCURACY_VALUE',
'Maximum model space distance between geometric entities at asserted c
onnectivities');
#9547=UNCERTAINTY_MEASURE_WITH_UNIT(LENGTH_MEASURE(0.01),#9562,
'DISTANCE_ACCURACY_VALUE',
'Maximum model space distance between geometric entities at asserted c
onnectivities');
#9548=UNCERTAINTY_MEASURE_WITH_UNIT(LENGTH_MEASURE(0.01),#9562,
'DISTANCE_ACCURACY_VALUE',
'Maximum model space distance between geometric entities at asserted c
onnectivities');
#9549=UNCERTAINTY_MEASURE_WITH_UNIT(LENGTH_MEASURE(0.01),#9562,
'DISTANCE_ACCURACY_VALUE',
'Maximum model space distance between geometric entities at asserted c
onnectivities');
#9550=UNCERTAINTY_MEASURE_WITH_UNIT(LENGTH_MEASURE(0.01),#9562,
'DISTANCE_ACCURACY_VALUE',
'Maximum model space distance between geometric entities at asserted c
onnectivities');
#9551=UNCERTAINTY_MEASURE_WITH_UNIT(LENGTH_MEASURE(0.01),#9562,
'DISTANCE_ACCURACY_VALUE',
'Maximum model space distance between geometric entities at asserted c
onnectivities');
#9552=UNCERTAINTY_MEASURE_WITH_UNIT(LENGTH_MEASURE(0.01),#9562,
'DISTANCE_ACCURACY_VALUE',
'Maximum model space distance between geometric entities at asserted c
onnectivities');
#9553=UNCERTAINTY_MEASURE_WITH_UNIT(LENGTH_MEASURE(0.01),#9562,
'DISTANCE_ACCURACY_VALUE',
'Maximum model space distance between geometric entities at asserted c
onnectivities');
#9554=(
GEOMETRIC_REPRESENTATION_CONTEXT(3)
GLOBAL_UNCERTAINTY_ASSIGNED_CONTEXT((#9546))
GLOBAL_UNIT_ASSIGNED_CONTEXT((#9562,#9564,#9565))
REPRESENTATION_CONTEXT('','3D')
);
#9555=(
GEOMETRIC_REPRESENTATION_CONTEXT(3)
GLOBAL_UNCERTAINTY_ASSIGNED_CONTEXT((#9547))
GLOBAL_UNIT_ASSIGNED_CONTEXT((#9562,#9564,#9565))
REPRESENTATION_CONTEXT('','3D')
);
#9556=(
GEOMETRIC_REPRESENTATION_CONTEXT(3)
GLOBAL_UNCERTAINTY_ASSIGNED_CONTEXT((#9548))
GLOBAL_UNIT_ASSIGNED_CONTEXT((#9562,#9564,#9565))
REPRESENTATION_CONTEXT('','3D')
);
#9557=(
GEOMETRIC_REPRESENTATION_CONTEXT(3)
GLOBAL_UNCERTAINTY_ASSIGNED_CONTEXT((#9549))
GLOBAL_UNIT_ASSIGNED_CONTEXT((#9562,#9564,#9565))
REPRESENTATION_CONTEXT('','3D')
);
#9558=(
GEOMETRIC_REPRESENTATION_CONTEXT(3)
GLOBAL_UNCERTAINTY_ASSIGNED_CONTEXT((#9550))
GLOBAL_UNIT_ASSIGNED_CONTEXT((#9562,#9564,#9565))
REPRESENTATION_CONTEXT('','3D')
);
#9559=(
GEOMETRIC_REPRESENTATION_CONTEXT(3)
GLOBAL_UNCERTAINTY_ASSIGNED_CONTEXT((#9551))
GLOBAL_UNIT_ASSIGNED_CONTEXT((#9562,#9564,#9565))
REPRESENTATION_CONTEXT('','3D')
);
#9560=(
GEOMETRIC_REPRESENTATION_CONTEXT(3)
GLOBAL_UNCERTAINTY_ASSIGNED_CONTEXT((#9552))
GLOBAL_UNIT_ASSIGNED_CONTEXT((#9562,#9564,#9565))
REPRESENTATION_CONTEXT('','3D')
);
#9561=(
GEOMETRIC_REPRESENTATION_CONTEXT(3)
GLOBAL_UNCERTAINTY_ASSIGNED_CONTEXT((#9553))
GLOBAL_UNIT_ASSIGNED_CONTEXT((#9562,#9564,#9565))
REPRESENTATION_CONTEXT('','3D')
);
#9562=(
LENGTH_UNIT()
NAMED_UNIT(*)
SI_UNIT(.MILLI.,.METRE.)
);
#9563=(
LENGTH_UNIT()
NAMED_UNIT(*)
SI_UNIT($,.METRE.)
);
#9564=(
NAMED_UNIT(*)
PLANE_ANGLE_UNIT()
SI_UNIT($,.RADIAN.)
);
#9565=(
NAMED_UNIT(*)
SI_UNIT($,.STERADIAN.)
SOLID_ANGLE_UNIT()
);
#9566=SHAPE_DEFINITION_REPRESENTATION(#9573,#9586);
#9567=SHAPE_DEFINITION_REPRESENTATION(#9574,#9587);
#9568=SHAPE_DEFINITION_REPRESENTATION(#9575,#9588);
#9569=SHAPE_DEFINITION_REPRESENTATION(#9576,#9589);
#9570=SHAPE_DEFINITION_REPRESENTATION(#9577,#9590);
#9571=SHAPE_DEFINITION_REPRESENTATION(#9578,#9591);
#9572=SHAPE_DEFINITION_REPRESENTATION(#9579,#9592);
#9573=PRODUCT_DEFINITION_SHAPE('',$,#9594);
#9574=PRODUCT_DEFINITION_SHAPE('',$,#9595);
#9575=PRODUCT_DEFINITION_SHAPE('',$,#9596);
#9576=PRODUCT_DEFINITION_SHAPE('',$,#9597);
#9577=PRODUCT_DEFINITION_SHAPE('',$,#9598);
#9578=PRODUCT_DEFINITION_SHAPE('',$,#9599);
#9579=PRODUCT_DEFINITION_SHAPE('',$,#9600);
#9580=PRODUCT_DEFINITION_SHAPE($,$,#29);
#9581=PRODUCT_DEFINITION_SHAPE($,$,#30);
#9582=PRODUCT_DEFINITION_SHAPE($,$,#31);
#9583=PRODUCT_DEFINITION_SHAPE($,$,#32);
#9584=PRODUCT_DEFINITION_SHAPE($,$,#33);
#9585=PRODUCT_DEFINITION_SHAPE($,$,#34);
#9586=SHAPE_REPRESENTATION('',(#2478,#2690,#2691,#2692,#2693,#2694,#2695),
#9554);
#9587=SHAPE_REPRESENTATION('',(#2479),#9555);
#9588=SHAPE_REPRESENTATION('',(#2539),#9556);
#9589=SHAPE_REPRESENTATION('',(#2590),#9557);
#9590=SHAPE_REPRESENTATION('',(#2613),#9558);
#9591=SHAPE_REPRESENTATION('',(#2678),#9559);
#9592=SHAPE_REPRESENTATION('',(#2684),#9560);
#9593=PRODUCT_DEFINITION_CONTEXT('part definition',#9616,'design');
#9594=PRODUCT_DEFINITION('Corkscrew Opener','TAS-004',#9601,#9593);
#9595=PRODUCT_DEFINITION('Handle','Handle',#9602,#9593);
#9596=PRODUCT_DEFINITION('fulcrum','fulcrum',#9603,#9593);
#9597=PRODUCT_DEFINITION('Central Grooved Worm Spiral Wire',
'Central Grooved Worm Spiral Wire',#9604,#9593);
#9598=PRODUCT_DEFINITION('foil cutter','foil cutter',#9605,#9593);
#9599=PRODUCT_DEFINITION('pin 1','pin 1',#9606,#9593);
#9600=PRODUCT_DEFINITION('pin 2','pin 2',#9607,#9593);
#9601=PRODUCT_DEFINITION_FORMATION('',$,#9618);
#9602=PRODUCT_DEFINITION_FORMATION('',$,#9619);
#9603=PRODUCT_DEFINITION_FORMATION('',$,#9620);
#9604=PRODUCT_DEFINITION_FORMATION('',$,#9621);
#9605=PRODUCT_DEFINITION_FORMATION('',$,#9622);
#9606=PRODUCT_DEFINITION_FORMATION('',$,#9623);
#9607=PRODUCT_DEFINITION_FORMATION('',$,#9624);
#9608=PRODUCT_RELATED_PRODUCT_CATEGORY('TAS-004','TAS-004',(#9618));
#9609=PRODUCT_RELATED_PRODUCT_CATEGORY('Handle','Handle',(#9619));
#9610=PRODUCT_RELATED_PRODUCT_CATEGORY('fulcrum','fulcrum',(#9620));
#9611=PRODUCT_RELATED_PRODUCT_CATEGORY(
'Central Grooved Worm Spiral Wire','Central Grooved Worm Spiral Wire',(#9621));
#9612=PRODUCT_RELATED_PRODUCT_CATEGORY('foil cutter','foil cutter',(#9622));
#9613=PRODUCT_RELATED_PRODUCT_CATEGORY('pin 1','pin 1',(#9623));
#9614=PRODUCT_RELATED_PRODUCT_CATEGORY('pin 2','pin 2',(#9624));
#9615=APPLICATION_PROTOCOL_DEFINITION('international standard',
'automotive_design',2009,#9616);
#9616=APPLICATION_CONTEXT(
'Core Data for Automotive Mechanical Design Process');
#9617=PRODUCT_CONTEXT('part definition',#9616,'mechanical');
#9618=PRODUCT('Corkscrew Opener','TAS-004','STEP AP214',(#9617));
#9619=PRODUCT('Handle','Handle',$,(#9617));
#9620=PRODUCT('fulcrum','fulcrum',$,(#9617));
#9621=PRODUCT('Central Grooved Worm Spiral Wire',
'Central Grooved Worm Spiral Wire',$,(#9617));
#9622=PRODUCT('foil cutter','foil cutter',$,(#9617));
#9623=PRODUCT('pin 1','pin 1',$,(#9617));
#9624=PRODUCT('pin 2','pin 2',$,(#9617));
#9625=PRESENTATION_STYLE_ASSIGNMENT((#9630));
#9626=PRESENTATION_STYLE_ASSIGNMENT((#9631));
#9627=PRESENTATION_STYLE_ASSIGNMENT((#9632));
#9628=PRESENTATION_STYLE_ASSIGNMENT((#9633));
#9629=PRESENTATION_STYLE_ASSIGNMENT((#9634));
#9630=SURFACE_STYLE_USAGE(.BOTH.,#9635);
#9631=SURFACE_STYLE_USAGE(.BOTH.,#9636);
#9632=SURFACE_STYLE_USAGE(.BOTH.,#9637);
#9633=SURFACE_STYLE_USAGE(.BOTH.,#9638);
#9634=SURFACE_STYLE_USAGE(.BOTH.,#9639);
#9635=SURFACE_SIDE_STYLE('',(#9640));
#9636=SURFACE_SIDE_STYLE('',(#9641));
#9637=SURFACE_SIDE_STYLE('',(#9642));
#9638=SURFACE_SIDE_STYLE('',(#9643));
#9639=SURFACE_SIDE_STYLE('',(#9644));
#9640=SURFACE_STYLE_FILL_AREA(#9645);
#9641=SURFACE_STYLE_FILL_AREA(#9646);
#9642=SURFACE_STYLE_FILL_AREA(#9647);
#9643=SURFACE_STYLE_FILL_AREA(#9648);
#9644=SURFACE_STYLE_FILL_AREA(#9649);
#9645=FILL_AREA_STYLE('Steel - Satin',(#9650));
#9646=FILL_AREA_STYLE('Opaque(61,176,222)',(#9651));
#9647=FILL_AREA_STYLE('Opaque(97,158,199)',(#9652));
#9648=FILL_AREA_STYLE('Opaque(227,224,212)',(#9653));
#9649=FILL_AREA_STYLE('Opaque(122,133,145)',(#9654));
#9650=FILL_AREA_STYLE_COLOUR('Steel - Satin',#9655);
#9651=FILL_AREA_STYLE_COLOUR('Opaque(61,176,222)',#9656);
#9652=FILL_AREA_STYLE_COLOUR('Opaque(97,158,199)',#9657);
#9653=FILL_AREA_STYLE_COLOUR('Opaque(227,224,212)',#9658);
#9654=FILL_AREA_STYLE_COLOUR('Opaque(122,133,145)',#9659);
#9655=COLOUR_RGB('Steel - Satin',0.627450980392157,0.627450980392157,0.627450980392157);
#9656=COLOUR_RGB('Opaque(61,176,222)',0.23921568627451,0.690196078431373,
0.870588235294118);
#9657=COLOUR_RGB('Opaque(97,158,199)',0.380392156862745,0.619607843137255,
0.780392156862745);
#9658=COLOUR_RGB('Opaque(227,224,212)',0.890196078431372,0.87843137254902,
0.831372549019608);
#9659=COLOUR_RGB('Opaque(122,133,145)',0.47843137254902,0.52156862745098,
0.568627450980392);
ENDSEC;
END-ISO-10303-21;
